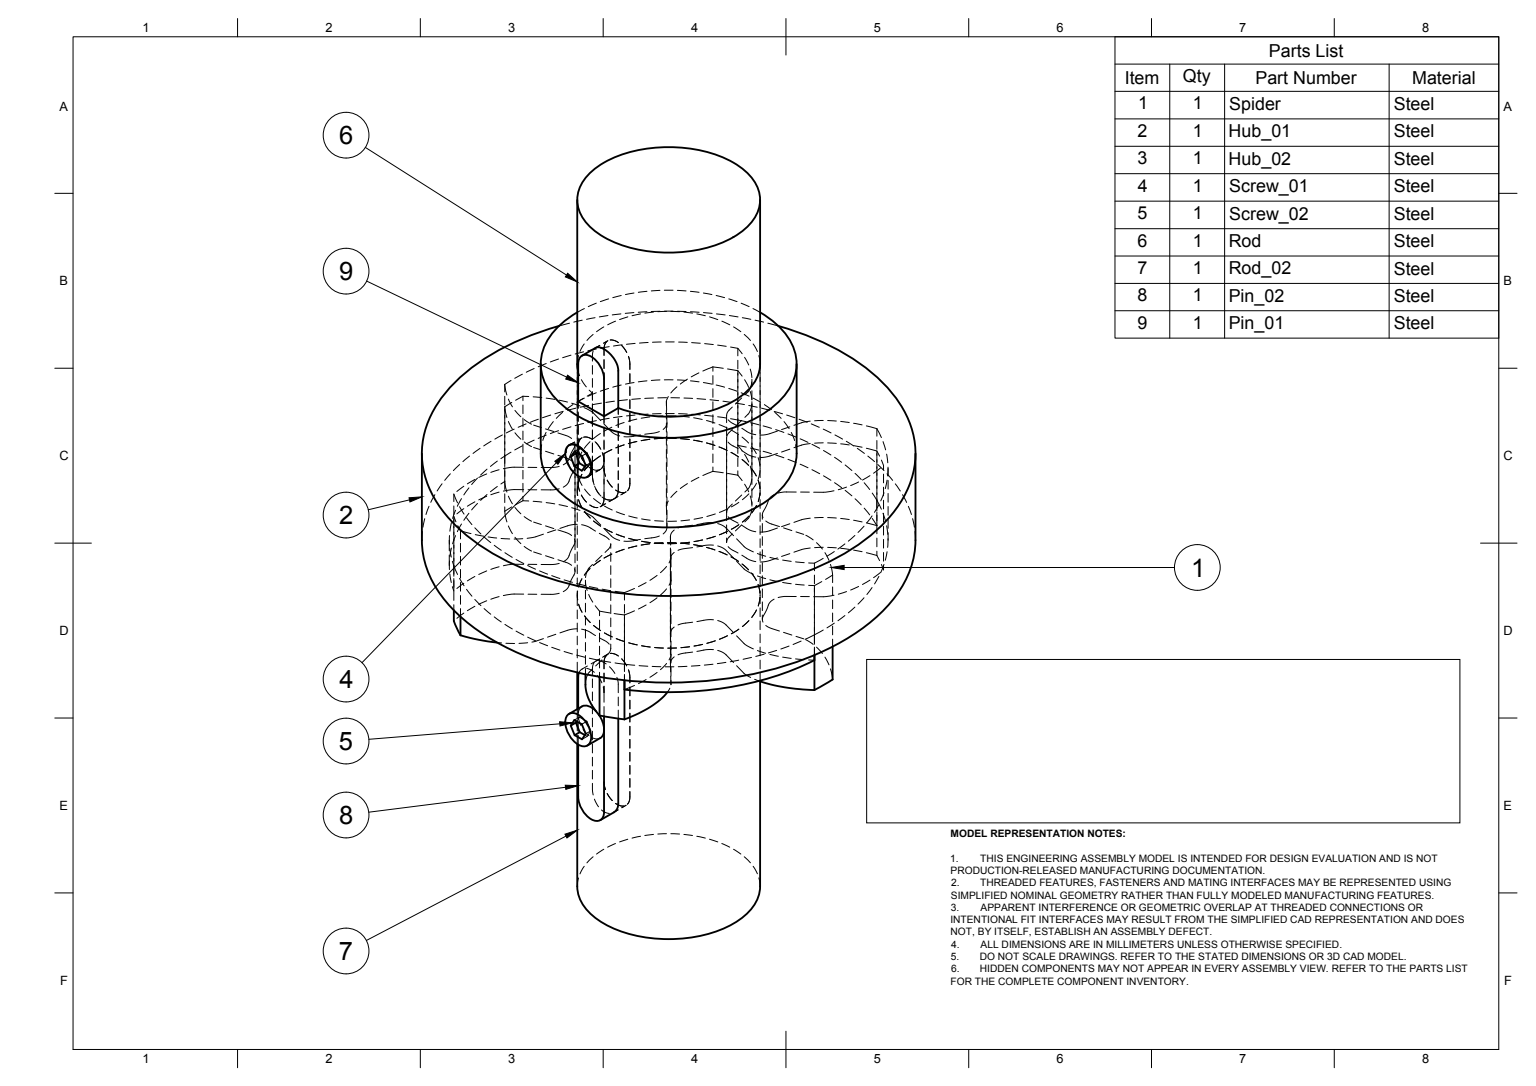
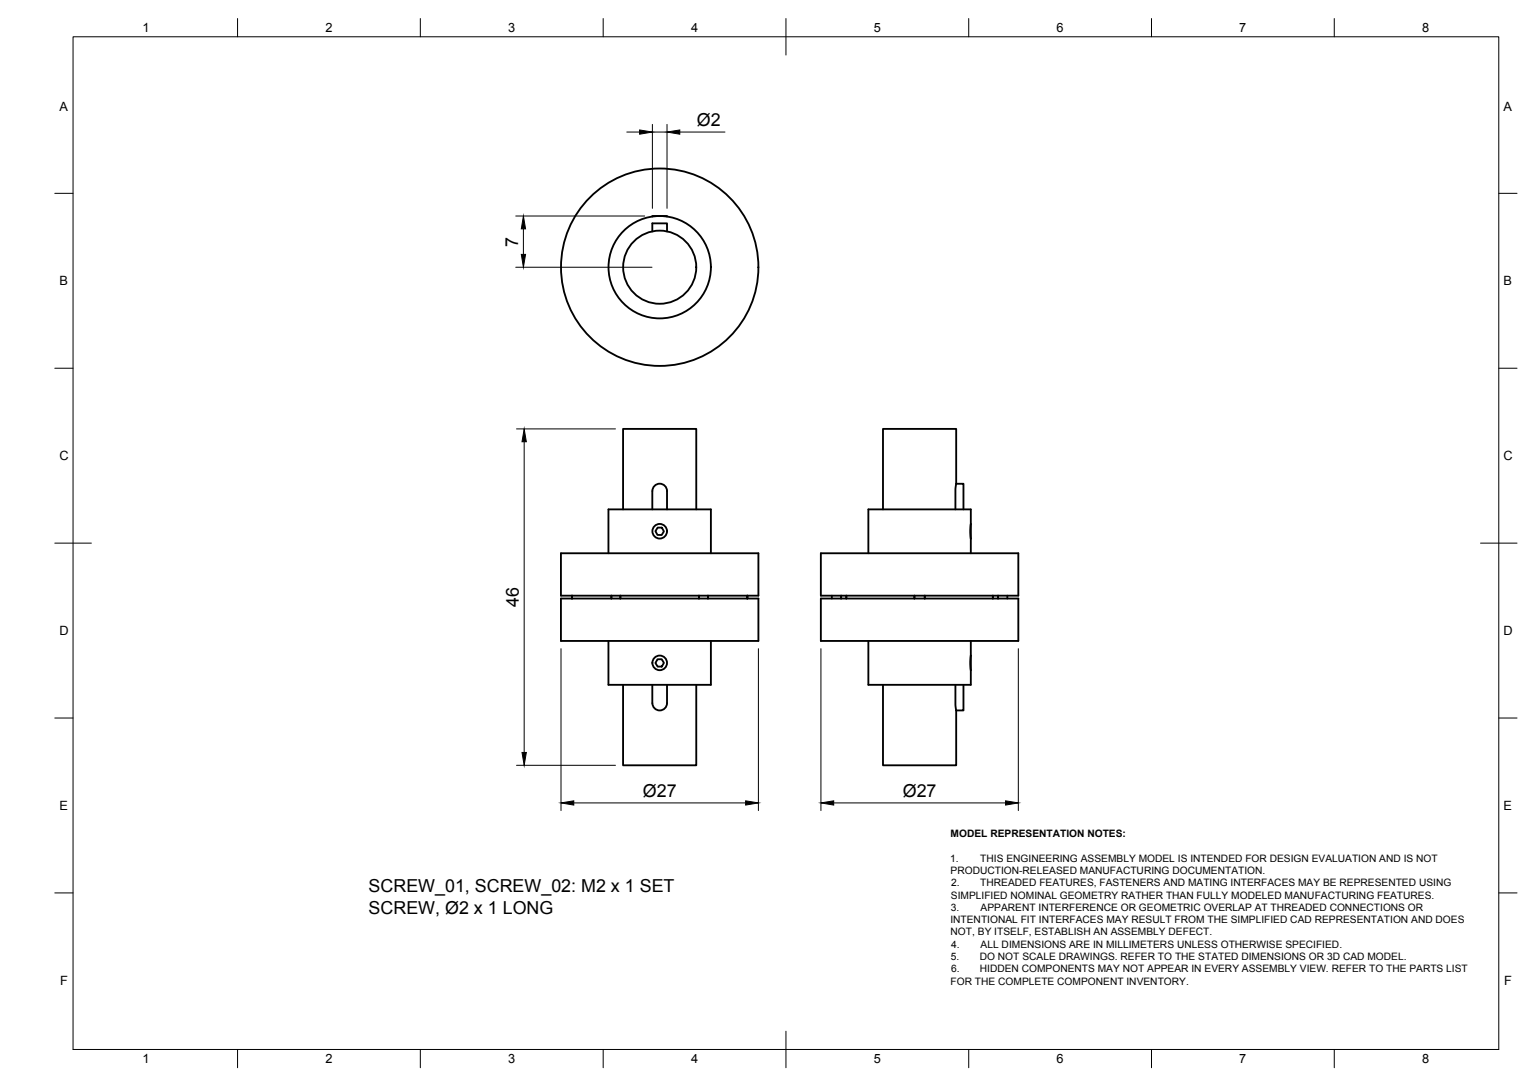
ISO-10303-21;
HEADER;
/* Generated by software containing ST-Developer
 * from STEP Tools, Inc. (www.steptools.com) 
 */

FILE_DESCRIPTION(
/* description */ (''),
/* implementation_level */ '2;1');

FILE_NAME(
/* name */ 'BR-255',
/* time_stamp */ '2026-10-05T21:34:53-07:00',
/* author */ (''),
/* organization */ (''),
/* preprocessor_version */ 'ST-DEVELOPER v20.2',
/* originating_system */ 'Autodesk Translation Framework v15.15.0.0',
/* authorisation */ '');

FILE_SCHEMA (('AUTOMOTIVE_DESIGN { 1 0 10303 214 3 1 1 }'));
ENDSEC;

DATA;
#10=MECHANICAL_DESIGN_GEOMETRIC_PRESENTATION_REPRESENTATION('',(#65,#66,
#67,#68,#69,#70,#71,#72,#73),#9822);
#11=ITEM_DEFINED_TRANSFORMATION($,$,#3398,#3718);
#12=ITEM_DEFINED_TRANSFORMATION($,$,#3488,#3719);
#13=ITEM_DEFINED_TRANSFORMATION($,$,#3566,#3720);
#14=ITEM_DEFINED_TRANSFORMATION($,$,#3644,#3721);
#15=ITEM_DEFINED_TRANSFORMATION($,$,#3657,#3722);
#16=ITEM_DEFINED_TRANSFORMATION($,$,#3670,#3723);
#17=ITEM_DEFINED_TRANSFORMATION($,$,#3683,#3724);
#18=ITEM_DEFINED_TRANSFORMATION($,$,#3696,#3725);
#19=ITEM_DEFINED_TRANSFORMATION($,$,#3707,#3726);
#20=(
REPRESENTATION_RELATIONSHIP($,$,#9857,#9856)
REPRESENTATION_RELATIONSHIP_WITH_TRANSFORMATION(#11)
SHAPE_REPRESENTATION_RELATIONSHIP()
);
#21=(
REPRESENTATION_RELATIONSHIP($,$,#9858,#9856)
REPRESENTATION_RELATIONSHIP_WITH_TRANSFORMATION(#12)
SHAPE_REPRESENTATION_RELATIONSHIP()
);
#22=(
REPRESENTATION_RELATIONSHIP($,$,#9859,#9856)
REPRESENTATION_RELATIONSHIP_WITH_TRANSFORMATION(#13)
SHAPE_REPRESENTATION_RELATIONSHIP()
);
#23=(
REPRESENTATION_RELATIONSHIP($,$,#9860,#9856)
REPRESENTATION_RELATIONSHIP_WITH_TRANSFORMATION(#14)
SHAPE_REPRESENTATION_RELATIONSHIP()
);
#24=(
REPRESENTATION_RELATIONSHIP($,$,#9861,#9856)
REPRESENTATION_RELATIONSHIP_WITH_TRANSFORMATION(#15)
SHAPE_REPRESENTATION_RELATIONSHIP()
);
#25=(
REPRESENTATION_RELATIONSHIP($,$,#9862,#9856)
REPRESENTATION_RELATIONSHIP_WITH_TRANSFORMATION(#16)
SHAPE_REPRESENTATION_RELATIONSHIP()
);
#26=(
REPRESENTATION_RELATIONSHIP($,$,#9863,#9856)
REPRESENTATION_RELATIONSHIP_WITH_TRANSFORMATION(#17)
SHAPE_REPRESENTATION_RELATIONSHIP()
);
#27=(
REPRESENTATION_RELATIONSHIP($,$,#9864,#9856)
REPRESENTATION_RELATIONSHIP_WITH_TRANSFORMATION(#18)
SHAPE_REPRESENTATION_RELATIONSHIP()
);
#28=(
REPRESENTATION_RELATIONSHIP($,$,#9865,#9856)
REPRESENTATION_RELATIONSHIP_WITH_TRANSFORMATION(#19)
SHAPE_REPRESENTATION_RELATIONSHIP()
);
#29=CONTEXT_DEPENDENT_SHAPE_REPRESENTATION(#20,#9847);
#30=CONTEXT_DEPENDENT_SHAPE_REPRESENTATION(#21,#9848);
#31=CONTEXT_DEPENDENT_SHAPE_REPRESENTATION(#22,#9849);
#32=CONTEXT_DEPENDENT_SHAPE_REPRESENTATION(#23,#9850);
#33=CONTEXT_DEPENDENT_SHAPE_REPRESENTATION(#24,#9851);
#34=CONTEXT_DEPENDENT_SHAPE_REPRESENTATION(#25,#9852);
#35=CONTEXT_DEPENDENT_SHAPE_REPRESENTATION(#26,#9853);
#36=CONTEXT_DEPENDENT_SHAPE_REPRESENTATION(#27,#9854);
#37=CONTEXT_DEPENDENT_SHAPE_REPRESENTATION(#28,#9855);
#38=NEXT_ASSEMBLY_USAGE_OCCURRENCE('Spider:1','Spider:1','Spider:1',#9867,
#9868,'Spider:1');
#39=NEXT_ASSEMBLY_USAGE_OCCURRENCE('Hub_01:1','Hub_01:1','Hub_01:1',#9867,
#9869,'Hub_01:1');
#40=NEXT_ASSEMBLY_USAGE_OCCURRENCE('Hub_02:1','Hub_02:1','Hub_02:1',#9867,
#9870,'Hub_02:1');
#41=NEXT_ASSEMBLY_USAGE_OCCURRENCE('Screw_01:1','Screw_01:1',
'Screw_01:1',#9867,#9871,'Screw_01:1');
#42=NEXT_ASSEMBLY_USAGE_OCCURRENCE('Screw_02:1','Screw_02:1',
'Screw_02:1',#9867,#9872,'Screw_02:1');
#43=NEXT_ASSEMBLY_USAGE_OCCURRENCE('Rod:1','Rod:1','Rod:1',#9867,#9873,
'Rod:1');
#44=NEXT_ASSEMBLY_USAGE_OCCURRENCE('Rod_02:1','Rod_02:1','Rod_02:1',#9867,
#9874,'Rod_02:1');
#45=NEXT_ASSEMBLY_USAGE_OCCURRENCE('Pin_02:1','Pin_02:1','Pin_02:1',#9867,
#9875,'Pin_02:1');
#46=NEXT_ASSEMBLY_USAGE_OCCURRENCE('Pin_01:1','Pin_01:1','Pin_01:1',#9867,
#9876,'Pin_01:1');
#47=SHAPE_REPRESENTATION_RELATIONSHIP('SRR','None',#9857,#56);
#48=SHAPE_REPRESENTATION_RELATIONSHIP('SRR','None',#9858,#57);
#49=SHAPE_REPRESENTATION_RELATIONSHIP('SRR','None',#9859,#58);
#50=SHAPE_REPRESENTATION_RELATIONSHIP('SRR','None',#9860,#59);
#51=SHAPE_REPRESENTATION_RELATIONSHIP('SRR','None',#9861,#60);
#52=SHAPE_REPRESENTATION_RELATIONSHIP('SRR','None',#9862,#61);
#53=SHAPE_REPRESENTATION_RELATIONSHIP('SRR','None',#9863,#62);
#54=SHAPE_REPRESENTATION_RELATIONSHIP('SRR','None',#9864,#63);
#55=SHAPE_REPRESENTATION_RELATIONSHIP('SRR','None',#9865,#64);
#56=ADVANCED_BREP_SHAPE_REPRESENTATION('',(#74),#9813);
#57=ADVANCED_BREP_SHAPE_REPRESENTATION('',(#75),#9814);
#58=ADVANCED_BREP_SHAPE_REPRESENTATION('',(#76),#9815);
#59=ADVANCED_BREP_SHAPE_REPRESENTATION('',(#77),#9816);
#60=ADVANCED_BREP_SHAPE_REPRESENTATION('',(#78),#9817);
#61=ADVANCED_BREP_SHAPE_REPRESENTATION('',(#79),#9818);
#62=ADVANCED_BREP_SHAPE_REPRESENTATION('',(#80),#9819);
#63=ADVANCED_BREP_SHAPE_REPRESENTATION('',(#81),#9820);
#64=ADVANCED_BREP_SHAPE_REPRESENTATION('',(#82),#9821);
#65=STYLED_ITEM('',(#9911),#74);
#66=STYLED_ITEM('',(#9911),#75);
#67=STYLED_ITEM('',(#9911),#76);
#68=STYLED_ITEM('',(#9912),#77);
#69=STYLED_ITEM('',(#9912),#78);
#70=STYLED_ITEM('',(#9912),#79);
#71=STYLED_ITEM('',(#9912),#80);
#72=STYLED_ITEM('',(#9912),#81);
#73=STYLED_ITEM('',(#9912),#82);
#74=MANIFOLD_SOLID_BREP('Body1',#3288);
#75=MANIFOLD_SOLID_BREP('Body1',#3289);
#76=MANIFOLD_SOLID_BREP('Body1',#3290);
#77=MANIFOLD_SOLID_BREP('Body1',#3291);
#78=MANIFOLD_SOLID_BREP('Body1',#3292);
#79=MANIFOLD_SOLID_BREP('Body1',#3293);
#80=MANIFOLD_SOLID_BREP('Body1',#3294);
#81=MANIFOLD_SOLID_BREP('Body1',#3295);
#82=MANIFOLD_SOLID_BREP('Body1',#3296);
#83=FACE_BOUND('',#486,.T.);
#84=FACE_BOUND('',#500,.T.);
#85=FACE_BOUND('',#514,.T.);
#86=FACE_BOUND('',#518,.T.);
#87=FACE_BOUND('',#520,.T.);
#88=FACE_BOUND('',#522,.T.);
#89=FACE_BOUND('',#525,.T.);
#90=FACE_BOUND('',#562,.T.);
#91=FACE_BOUND('',#566,.T.);
#92=FACE_BOUND('',#568,.T.);
#93=FACE_BOUND('',#570,.T.);
#94=FACE_BOUND('',#573,.T.);
#95=FACE_BOUND('',#608,.T.);
#96=FACE_BOUND('',#619,.T.);
#97=FACE_BOUND('',#628,.T.);
#98=FACE_BOUND('',#637,.T.);
#99=B_SPLINE_CURVE_WITH_KNOTS('',5,(#4949,#4950,#4951,#4952,#4953,#4954,
#4955,#4956,#4957,#4958,#4959,#4960,#4961,#4962,#4963,#4964,#4965,#4966,
#4967,#4968,#4969,#4970,#4971,#4972,#4973,#4974,#4975,#4976,#4977,#4978,
#4979,#4980,#4981,#4982,#4983,#4984,#4985,#4986,#4987,#4988,#4989,#4990,
#4991,#4992,#4993,#4994,#4995,#4996,#4997,#4998,#4999,#5000,#5001,#5002,
#5003,#5004,#5005,#5006,#5007,#5008,#5009,#5010,#5011,#5012,#5013,#5014,
#5015,#5016,#5017,#5018,#5019,#5020,#5021,#5022,#5023),.UNSPECIFIED.,.F.,
 .F.,(6,1,1,1,1,1,1,1,1,1,1,1,1,1,1,1,1,1,1,1,1,1,1,1,1,1,1,1,1,1,1,1,1,
1,1,1,1,1,1,1,1,1,1,1,1,1,1,1,1,1,1,1,1,1,1,1,1,1,1,1,1,1,1,1,1,1,1,1,1,
1,6),(-1.,-0.985714285714284,-0.97142857142857,-0.957142857142856,-0.942857142857141,
-0.928571428571427,-0.914285714285713,-0.899999999999999,-0.885714285714284,
-0.87142857142857,-0.857142857142856,-0.842857142857142,-0.828571428571428,
-0.814285714285713,-0.799999999999999,-0.785714285714285,-0.771428571428571,
-0.757142857142856,-0.742857142857142,-0.728571428571428,-0.714285714285714,
-0.699999999999999,-0.685714285714285,-0.671428571428571,-0.657142857142857,
-0.642857142857142,-0.628571428571428,-0.614285714285714,-0.6,-0.585714285714286,
-0.571428571428571,-0.557142857142857,-0.542857142857143,-0.528571428571429,
-0.514285714285714,-0.5,-0.485714285714286,-0.471428571428572,-0.457142857142857,
-0.442857142857143,-0.428571428571429,-0.414285714285714,-0.4,-0.385714285714286,
-0.371428571428571,-0.357142857142857,-0.342857142857143,-0.328571428571429,
-0.314285714285714,-0.3,-0.285714285714286,-0.271428571428571,-0.257142857142857,
-0.242857142857143,-0.228571428571429,-0.214285714285714,-0.2,-0.185714285714286,
-0.171428571428571,-0.157142857142857,-0.142857142857143,-0.128571428571429,
-0.114285714285714,-0.1,-0.0857142857142857,-0.0714285714285714,-0.0571428571428571,
-0.0428571428571429,-0.0285714285714286,-0.0142857142857143,0.),
 .UNSPECIFIED.);
#100=B_SPLINE_CURVE_WITH_KNOTS('',5,(#5025,#5026,#5027,#5028,#5029,#5030,
#5031,#5032,#5033,#5034,#5035,#5036,#5037,#5038,#5039,#5040,#5041,#5042,
#5043,#5044,#5045,#5046,#5047,#5048,#5049,#5050,#5051,#5052,#5053,#5054,
#5055,#5056,#5057,#5058,#5059,#5060,#5061,#5062,#5063,#5064,#5065,#5066,
#5067,#5068,#5069,#5070,#5071,#5072,#5073,#5074,#5075,#5076,#5077,#5078,
#5079,#5080,#5081,#5082,#5083,#5084,#5085,#5086,#5087,#5088,#5089,#5090,
#5091,#5092,#5093,#5094,#5095,#5096,#5097,#5098,#5099),.UNSPECIFIED.,.F.,
 .F.,(6,1,1,1,1,1,1,1,1,1,1,1,1,1,1,1,1,1,1,1,1,1,1,1,1,1,1,1,1,1,1,1,1,
1,1,1,1,1,1,1,1,1,1,1,1,1,1,1,1,1,1,1,1,1,1,1,1,1,1,1,1,1,1,1,1,1,1,1,1,
1,6),(-1.,-0.985714285714284,-0.97142857142857,-0.957142857142856,-0.942857142857141,
-0.928571428571427,-0.914285714285713,-0.899999999999999,-0.885714285714284,
-0.87142857142857,-0.857142857142856,-0.842857142857142,-0.828571428571428,
-0.814285714285713,-0.799999999999999,-0.785714285714285,-0.771428571428571,
-0.757142857142856,-0.742857142857142,-0.728571428571428,-0.714285714285714,
-0.699999999999999,-0.685714285714285,-0.671428571428571,-0.657142857142857,
-0.642857142857142,-0.628571428571428,-0.614285714285714,-0.6,-0.585714285714286,
-0.571428571428571,-0.557142857142857,-0.542857142857143,-0.528571428571429,
-0.514285714285714,-0.5,-0.485714285714286,-0.471428571428572,-0.457142857142857,
-0.442857142857143,-0.428571428571429,-0.414285714285714,-0.4,-0.385714285714286,
-0.371428571428571,-0.357142857142857,-0.342857142857143,-0.328571428571429,
-0.314285714285714,-0.3,-0.285714285714286,-0.271428571428571,-0.257142857142857,
-0.242857142857143,-0.228571428571429,-0.214285714285714,-0.2,-0.185714285714286,
-0.171428571428571,-0.157142857142857,-0.142857142857143,-0.128571428571429,
-0.114285714285714,-0.1,-0.0857142857142857,-0.0714285714285714,-0.0571428571428571,
-0.0428571428571429,-0.0285714285714286,-0.0142857142857143,0.),
 .UNSPECIFIED.);
#101=B_SPLINE_CURVE_WITH_KNOTS('',5,(#5257,#5258,#5259,#5260,#5261,#5262,
#5263,#5264,#5265,#5266,#5267,#5268,#5269,#5270,#5271,#5272,#5273,#5274,
#5275,#5276,#5277,#5278,#5279,#5280,#5281,#5282,#5283,#5284,#5285,#5286,
#5287,#5288,#5289,#5290,#5291,#5292,#5293,#5294,#5295,#5296,#5297,#5298,
#5299,#5300,#5301,#5302,#5303,#5304,#5305,#5306,#5307,#5308,#5309,#5310,
#5311,#5312,#5313,#5314,#5315,#5316,#5317,#5318,#5319,#5320,#5321,#5322,
#5323,#5324,#5325,#5326,#5327,#5328,#5329,#5330,#5331),.UNSPECIFIED.,.F.,
 .F.,(6,1,1,1,1,1,1,1,1,1,1,1,1,1,1,1,1,1,1,1,1,1,1,1,1,1,1,1,1,1,1,1,1,
1,1,1,1,1,1,1,1,1,1,1,1,1,1,1,1,1,1,1,1,1,1,1,1,1,1,1,1,1,1,1,1,1,1,1,1,
1,6),(0.,0.0142857142857143,0.0285714285714286,0.0428571428571429,0.0571428571428571,
0.0714285714285714,0.0857142857142857,0.1,0.114285714285714,0.128571428571429,
0.142857142857143,0.157142857142857,0.171428571428571,0.185714285714286,
0.2,0.214285714285714,0.228571428571429,0.242857142857143,0.257142857142857,
0.271428571428571,0.285714285714286,0.3,0.314285714285714,0.328571428571429,
0.342857142857143,0.357142857142857,0.371428571428571,0.385714285714286,
0.4,0.414285714285714,0.428571428571429,0.442857142857143,0.457142857142857,
0.471428571428572,0.485714285714286,0.5,0.514285714285714,0.528571428571429,
0.542857142857143,0.557142857142857,0.571428571428571,0.585714285714286,
0.6,0.614285714285714,0.628571428571428,0.642857142857142,0.657142857142857,
0.671428571428571,0.685714285714285,0.699999999999999,0.714285714285714,
0.728571428571428,0.742857142857142,0.757142857142856,0.771428571428571,
0.785714285714285,0.799999999999999,0.814285714285713,0.828571428571428,
0.842857142857142,0.857142857142856,0.87142857142857,0.885714285714284,
0.899999999999999,0.914285714285713,0.928571428571427,0.942857142857141,
0.957142857142856,0.97142857142857,0.985714285714284,1.),.UNSPECIFIED.);
#102=B_SPLINE_CURVE_WITH_KNOTS('',5,(#5332,#5333,#5334,#5335,#5336,#5337,
#5338,#5339,#5340,#5341,#5342,#5343,#5344,#5345,#5346,#5347,#5348,#5349,
#5350,#5351,#5352,#5353,#5354,#5355,#5356,#5357,#5358,#5359,#5360,#5361,
#5362,#5363,#5364,#5365,#5366,#5367,#5368,#5369,#5370,#5371,#5372,#5373,
#5374,#5375,#5376,#5377,#5378,#5379,#5380,#5381,#5382,#5383,#5384,#5385,
#5386,#5387,#5388,#5389,#5390,#5391,#5392,#5393,#5394,#5395,#5396,#5397,
#5398,#5399,#5400,#5401,#5402,#5403,#5404,#5405,#5406),.UNSPECIFIED.,.F.,
 .F.,(6,1,1,1,1,1,1,1,1,1,1,1,1,1,1,1,1,1,1,1,1,1,1,1,1,1,1,1,1,1,1,1,1,
1,1,1,1,1,1,1,1,1,1,1,1,1,1,1,1,1,1,1,1,1,1,1,1,1,1,1,1,1,1,1,1,1,1,1,1,
1,6),(0.,0.0142857142857143,0.0285714285714286,0.0428571428571429,0.0571428571428571,
0.0714285714285714,0.0857142857142857,0.1,0.114285714285714,0.128571428571429,
0.142857142857143,0.157142857142857,0.171428571428571,0.185714285714286,
0.2,0.214285714285714,0.228571428571429,0.242857142857143,0.257142857142857,
0.271428571428571,0.285714285714286,0.3,0.314285714285714,0.328571428571429,
0.342857142857143,0.357142857142857,0.371428571428571,0.385714285714286,
0.4,0.414285714285714,0.428571428571429,0.442857142857143,0.457142857142857,
0.471428571428572,0.485714285714286,0.5,0.514285714285714,0.528571428571429,
0.542857142857143,0.557142857142857,0.571428571428571,0.585714285714286,
0.6,0.614285714285714,0.628571428571428,0.642857142857142,0.657142857142857,
0.671428571428571,0.685714285714285,0.699999999999999,0.714285714285714,
0.728571428571428,0.742857142857142,0.757142857142856,0.771428571428571,
0.785714285714285,0.799999999999999,0.814285714285713,0.828571428571428,
0.842857142857142,0.857142857142856,0.87142857142857,0.885714285714284,
0.899999999999999,0.914285714285713,0.928571428571427,0.942857142857141,
0.957142857142856,0.97142857142857,0.985714285714284,1.),.UNSPECIFIED.);
#103=B_SPLINE_CURVE_WITH_KNOTS('',5,(#5558,#5559,#5560,#5561,#5562,#5563,
#5564,#5565,#5566,#5567,#5568,#5569,#5570,#5571,#5572,#5573,#5574,#5575,
#5576,#5577,#5578,#5579,#5580,#5581,#5582,#5583,#5584,#5585,#5586,#5587,
#5588,#5589,#5590,#5591,#5592,#5593,#5594,#5595,#5596,#5597,#5598,#5599,
#5600,#5601,#5602,#5603,#5604,#5605,#5606,#5607,#5608,#5609,#5610,#5611,
#5612,#5613,#5614,#5615,#5616,#5617,#5618,#5619,#5620,#5621,#5622,#5623,
#5624,#5625,#5626,#5627,#5628,#5629,#5630,#5631,#5632),.UNSPECIFIED.,.F.,
 .F.,(6,1,1,1,1,1,1,1,1,1,1,1,1,1,1,1,1,1,1,1,1,1,1,1,1,1,1,1,1,1,1,1,1,
1,1,1,1,1,1,1,1,1,1,1,1,1,1,1,1,1,1,1,1,1,1,1,1,1,1,1,1,1,1,1,1,1,1,1,1,
1,6),(-1.,-0.985714285714284,-0.97142857142857,-0.957142857142856,-0.942857142857141,
-0.928571428571427,-0.914285714285713,-0.899999999999999,-0.885714285714284,
-0.87142857142857,-0.857142857142856,-0.842857142857142,-0.828571428571428,
-0.814285714285713,-0.799999999999999,-0.785714285714285,-0.771428571428571,
-0.757142857142856,-0.742857142857142,-0.728571428571428,-0.714285714285714,
-0.699999999999999,-0.685714285714285,-0.671428571428571,-0.657142857142857,
-0.642857142857142,-0.628571428571428,-0.614285714285714,-0.6,-0.585714285714286,
-0.571428571428571,-0.557142857142857,-0.542857142857143,-0.528571428571429,
-0.514285714285714,-0.5,-0.485714285714286,-0.471428571428572,-0.457142857142857,
-0.442857142857143,-0.428571428571429,-0.414285714285714,-0.4,-0.385714285714286,
-0.371428571428571,-0.357142857142857,-0.342857142857143,-0.328571428571429,
-0.314285714285714,-0.3,-0.285714285714286,-0.271428571428571,-0.257142857142857,
-0.242857142857143,-0.228571428571429,-0.214285714285714,-0.2,-0.185714285714286,
-0.171428571428571,-0.157142857142857,-0.142857142857143,-0.128571428571429,
-0.114285714285714,-0.1,-0.0857142857142857,-0.0714285714285714,-0.0571428571428571,
-0.0428571428571429,-0.0285714285714286,-0.0142857142857143,0.),
 .UNSPECIFIED.);
#104=B_SPLINE_CURVE_WITH_KNOTS('',5,(#5634,#5635,#5636,#5637,#5638,#5639,
#5640,#5641,#5642,#5643,#5644,#5645,#5646,#5647,#5648,#5649,#5650,#5651,
#5652,#5653,#5654,#5655,#5656,#5657,#5658,#5659,#5660,#5661,#5662,#5663,
#5664,#5665,#5666,#5667,#5668,#5669,#5670,#5671,#5672,#5673,#5674,#5675,
#5676,#5677,#5678,#5679,#5680,#5681,#5682,#5683,#5684,#5685,#5686,#5687,
#5688,#5689,#5690,#5691,#5692,#5693,#5694,#5695,#5696,#5697,#5698,#5699,
#5700,#5701,#5702,#5703,#5704,#5705,#5706,#5707,#5708),.UNSPECIFIED.,.F.,
 .F.,(6,1,1,1,1,1,1,1,1,1,1,1,1,1,1,1,1,1,1,1,1,1,1,1,1,1,1,1,1,1,1,1,1,
1,1,1,1,1,1,1,1,1,1,1,1,1,1,1,1,1,1,1,1,1,1,1,1,1,1,1,1,1,1,1,1,1,1,1,1,
1,6),(-1.,-0.985714285714284,-0.97142857142857,-0.957142857142856,-0.942857142857141,
-0.928571428571427,-0.914285714285713,-0.899999999999999,-0.885714285714284,
-0.87142857142857,-0.857142857142856,-0.842857142857142,-0.828571428571428,
-0.814285714285713,-0.799999999999999,-0.785714285714285,-0.771428571428571,
-0.757142857142856,-0.742857142857142,-0.728571428571428,-0.714285714285714,
-0.699999999999999,-0.685714285714285,-0.671428571428571,-0.657142857142857,
-0.642857142857142,-0.628571428571428,-0.614285714285714,-0.6,-0.585714285714286,
-0.571428571428571,-0.557142857142857,-0.542857142857143,-0.528571428571429,
-0.514285714285714,-0.5,-0.485714285714286,-0.471428571428572,-0.457142857142857,
-0.442857142857143,-0.428571428571429,-0.414285714285714,-0.4,-0.385714285714286,
-0.371428571428571,-0.357142857142857,-0.342857142857143,-0.328571428571429,
-0.314285714285714,-0.3,-0.285714285714286,-0.271428571428571,-0.257142857142857,
-0.242857142857143,-0.228571428571429,-0.214285714285714,-0.2,-0.185714285714286,
-0.171428571428571,-0.157142857142857,-0.142857142857143,-0.128571428571429,
-0.114285714285714,-0.1,-0.0857142857142857,-0.0714285714285714,-0.0571428571428571,
-0.0428571428571429,-0.0285714285714286,-0.0142857142857143,0.),
 .UNSPECIFIED.);
#105=B_SPLINE_CURVE_WITH_KNOTS('',5,(#5866,#5867,#5868,#5869,#5870,#5871,
#5872,#5873,#5874,#5875,#5876,#5877,#5878,#5879,#5880,#5881,#5882,#5883,
#5884,#5885,#5886,#5887,#5888,#5889,#5890,#5891,#5892,#5893,#5894,#5895,
#5896,#5897,#5898,#5899,#5900,#5901,#5902,#5903,#5904,#5905,#5906,#5907,
#5908,#5909,#5910,#5911,#5912,#5913,#5914,#5915,#5916,#5917,#5918,#5919,
#5920,#5921,#5922,#5923,#5924,#5925,#5926,#5927,#5928,#5929,#5930,#5931,
#5932,#5933,#5934,#5935,#5936,#5937,#5938,#5939,#5940),.UNSPECIFIED.,.F.,
 .F.,(6,1,1,1,1,1,1,1,1,1,1,1,1,1,1,1,1,1,1,1,1,1,1,1,1,1,1,1,1,1,1,1,1,
1,1,1,1,1,1,1,1,1,1,1,1,1,1,1,1,1,1,1,1,1,1,1,1,1,1,1,1,1,1,1,1,1,1,1,1,
1,6),(0.,0.0142857142857143,0.0285714285714286,0.0428571428571429,0.0571428571428571,
0.0714285714285714,0.0857142857142857,0.1,0.114285714285714,0.128571428571429,
0.142857142857143,0.157142857142857,0.171428571428571,0.185714285714286,
0.2,0.214285714285714,0.228571428571429,0.242857142857143,0.257142857142857,
0.271428571428571,0.285714285714286,0.3,0.314285714285714,0.328571428571429,
0.342857142857143,0.357142857142857,0.371428571428571,0.385714285714286,
0.4,0.414285714285714,0.428571428571429,0.442857142857143,0.457142857142857,
0.471428571428572,0.485714285714286,0.5,0.514285714285714,0.528571428571429,
0.542857142857143,0.557142857142857,0.571428571428571,0.585714285714286,
0.6,0.614285714285714,0.628571428571428,0.642857142857142,0.657142857142857,
0.671428571428571,0.685714285714285,0.699999999999999,0.714285714285714,
0.728571428571428,0.742857142857142,0.757142857142856,0.771428571428571,
0.785714285714285,0.799999999999999,0.814285714285713,0.828571428571428,
0.842857142857142,0.857142857142856,0.87142857142857,0.885714285714284,
0.899999999999999,0.914285714285713,0.928571428571427,0.942857142857141,
0.957142857142856,0.97142857142857,0.985714285714284,1.),.UNSPECIFIED.);
#106=B_SPLINE_CURVE_WITH_KNOTS('',5,(#5941,#5942,#5943,#5944,#5945,#5946,
#5947,#5948,#5949,#5950,#5951,#5952,#5953,#5954,#5955,#5956,#5957,#5958,
#5959,#5960,#5961,#5962,#5963,#5964,#5965,#5966,#5967,#5968,#5969,#5970,
#5971,#5972,#5973,#5974,#5975,#5976,#5977,#5978,#5979,#5980,#5981,#5982,
#5983,#5984,#5985,#5986,#5987,#5988,#5989,#5990,#5991,#5992,#5993,#5994,
#5995,#5996,#5997,#5998,#5999,#6000,#6001,#6002,#6003,#6004,#6005,#6006,
#6007,#6008,#6009,#6010,#6011,#6012,#6013,#6014,#6015),.UNSPECIFIED.,.F.,
 .F.,(6,1,1,1,1,1,1,1,1,1,1,1,1,1,1,1,1,1,1,1,1,1,1,1,1,1,1,1,1,1,1,1,1,
1,1,1,1,1,1,1,1,1,1,1,1,1,1,1,1,1,1,1,1,1,1,1,1,1,1,1,1,1,1,1,1,1,1,1,1,
1,6),(0.,0.0142857142857143,0.0285714285714286,0.0428571428571429,0.0571428571428571,
0.0714285714285714,0.0857142857142857,0.1,0.114285714285714,0.128571428571429,
0.142857142857143,0.157142857142857,0.171428571428571,0.185714285714286,
0.2,0.214285714285714,0.228571428571429,0.242857142857143,0.257142857142857,
0.271428571428571,0.285714285714286,0.3,0.314285714285714,0.328571428571429,
0.342857142857143,0.357142857142857,0.371428571428571,0.385714285714286,
0.4,0.414285714285714,0.428571428571429,0.442857142857143,0.457142857142857,
0.471428571428572,0.485714285714286,0.5,0.514285714285714,0.528571428571429,
0.542857142857143,0.557142857142857,0.571428571428571,0.585714285714286,
0.6,0.614285714285714,0.628571428571428,0.642857142857142,0.657142857142857,
0.671428571428571,0.685714285714285,0.699999999999999,0.714285714285714,
0.728571428571428,0.742857142857142,0.757142857142856,0.771428571428571,
0.785714285714285,0.799999999999999,0.814285714285713,0.828571428571428,
0.842857142857142,0.857142857142856,0.87142857142857,0.885714285714284,
0.899999999999999,0.914285714285713,0.928571428571427,0.942857142857141,
0.957142857142856,0.97142857142857,0.985714285714284,1.),.UNSPECIFIED.);
#107=B_SPLINE_CURVE_WITH_KNOTS('',5,(#6167,#6168,#6169,#6170,#6171,#6172,
#6173,#6174,#6175,#6176,#6177,#6178,#6179,#6180,#6181,#6182,#6183,#6184,
#6185,#6186,#6187,#6188,#6189,#6190,#6191,#6192,#6193,#6194,#6195,#6196,
#6197,#6198,#6199,#6200,#6201,#6202,#6203,#6204,#6205,#6206,#6207,#6208,
#6209,#6210,#6211,#6212,#6213,#6214,#6215,#6216,#6217,#6218,#6219,#6220,
#6221,#6222,#6223,#6224,#6225,#6226,#6227,#6228,#6229,#6230,#6231,#6232,
#6233,#6234,#6235,#6236,#6237,#6238,#6239,#6240,#6241),.UNSPECIFIED.,.F.,
 .F.,(6,1,1,1,1,1,1,1,1,1,1,1,1,1,1,1,1,1,1,1,1,1,1,1,1,1,1,1,1,1,1,1,1,
1,1,1,1,1,1,1,1,1,1,1,1,1,1,1,1,1,1,1,1,1,1,1,1,1,1,1,1,1,1,1,1,1,1,1,1,
1,6),(-1.,-0.985714285714284,-0.97142857142857,-0.957142857142856,-0.942857142857141,
-0.928571428571427,-0.914285714285713,-0.899999999999999,-0.885714285714284,
-0.87142857142857,-0.857142857142856,-0.842857142857142,-0.828571428571428,
-0.814285714285713,-0.799999999999999,-0.785714285714285,-0.771428571428571,
-0.757142857142856,-0.742857142857142,-0.728571428571428,-0.714285714285714,
-0.699999999999999,-0.685714285714285,-0.671428571428571,-0.657142857142857,
-0.642857142857142,-0.628571428571428,-0.614285714285714,-0.6,-0.585714285714286,
-0.571428571428571,-0.557142857142857,-0.542857142857143,-0.528571428571429,
-0.514285714285714,-0.5,-0.485714285714286,-0.471428571428572,-0.457142857142857,
-0.442857142857143,-0.428571428571429,-0.414285714285714,-0.4,-0.385714285714286,
-0.371428571428571,-0.357142857142857,-0.342857142857143,-0.328571428571429,
-0.314285714285714,-0.3,-0.285714285714286,-0.271428571428571,-0.257142857142857,
-0.242857142857143,-0.228571428571429,-0.214285714285714,-0.2,-0.185714285714286,
-0.171428571428571,-0.157142857142857,-0.142857142857143,-0.128571428571429,
-0.114285714285714,-0.1,-0.0857142857142857,-0.0714285714285714,-0.0571428571428571,
-0.0428571428571429,-0.0285714285714286,-0.0142857142857143,0.),
 .UNSPECIFIED.);
#108=B_SPLINE_CURVE_WITH_KNOTS('',5,(#6243,#6244,#6245,#6246,#6247,#6248,
#6249,#6250,#6251,#6252,#6253,#6254,#6255,#6256,#6257,#6258,#6259,#6260,
#6261,#6262,#6263,#6264,#6265,#6266,#6267,#6268,#6269,#6270,#6271,#6272,
#6273,#6274,#6275,#6276,#6277,#6278,#6279,#6280,#6281,#6282,#6283,#6284,
#6285,#6286,#6287,#6288,#6289,#6290,#6291,#6292,#6293,#6294,#6295,#6296,
#6297,#6298,#6299,#6300,#6301,#6302,#6303,#6304,#6305,#6306,#6307,#6308,
#6309,#6310,#6311,#6312,#6313,#6314,#6315,#6316,#6317),.UNSPECIFIED.,.F.,
 .F.,(6,1,1,1,1,1,1,1,1,1,1,1,1,1,1,1,1,1,1,1,1,1,1,1,1,1,1,1,1,1,1,1,1,
1,1,1,1,1,1,1,1,1,1,1,1,1,1,1,1,1,1,1,1,1,1,1,1,1,1,1,1,1,1,1,1,1,1,1,1,
1,6),(-1.,-0.985714285714284,-0.97142857142857,-0.957142857142856,-0.942857142857141,
-0.928571428571427,-0.914285714285713,-0.899999999999999,-0.885714285714284,
-0.87142857142857,-0.857142857142856,-0.842857142857142,-0.828571428571428,
-0.814285714285713,-0.799999999999999,-0.785714285714285,-0.771428571428571,
-0.757142857142856,-0.742857142857142,-0.728571428571428,-0.714285714285714,
-0.699999999999999,-0.685714285714285,-0.671428571428571,-0.657142857142857,
-0.642857142857142,-0.628571428571428,-0.614285714285714,-0.6,-0.585714285714286,
-0.571428571428571,-0.557142857142857,-0.542857142857143,-0.528571428571429,
-0.514285714285714,-0.5,-0.485714285714286,-0.471428571428572,-0.457142857142857,
-0.442857142857143,-0.428571428571429,-0.414285714285714,-0.4,-0.385714285714286,
-0.371428571428571,-0.357142857142857,-0.342857142857143,-0.328571428571429,
-0.314285714285714,-0.3,-0.285714285714286,-0.271428571428571,-0.257142857142857,
-0.242857142857143,-0.228571428571429,-0.214285714285714,-0.2,-0.185714285714286,
-0.171428571428571,-0.157142857142857,-0.142857142857143,-0.128571428571429,
-0.114285714285714,-0.1,-0.0857142857142857,-0.0714285714285714,-0.0571428571428571,
-0.0428571428571429,-0.0285714285714286,-0.0142857142857143,0.),
 .UNSPECIFIED.);
#109=B_SPLINE_CURVE_WITH_KNOTS('',5,(#6475,#6476,#6477,#6478,#6479,#6480,
#6481,#6482,#6483,#6484,#6485,#6486,#6487,#6488,#6489,#6490,#6491,#6492,
#6493,#6494,#6495,#6496,#6497,#6498,#6499,#6500,#6501,#6502,#6503,#6504,
#6505,#6506,#6507,#6508,#6509,#6510,#6511,#6512,#6513,#6514,#6515,#6516,
#6517,#6518,#6519,#6520,#6521,#6522,#6523,#6524,#6525,#6526,#6527,#6528,
#6529,#6530,#6531,#6532,#6533,#6534,#6535,#6536,#6537,#6538,#6539,#6540,
#6541,#6542,#6543,#6544,#6545,#6546,#6547,#6548,#6549),.UNSPECIFIED.,.F.,
 .F.,(6,1,1,1,1,1,1,1,1,1,1,1,1,1,1,1,1,1,1,1,1,1,1,1,1,1,1,1,1,1,1,1,1,
1,1,1,1,1,1,1,1,1,1,1,1,1,1,1,1,1,1,1,1,1,1,1,1,1,1,1,1,1,1,1,1,1,1,1,1,
1,6),(0.,0.0142857142857143,0.0285714285714286,0.0428571428571429,0.0571428571428571,
0.0714285714285714,0.0857142857142857,0.1,0.114285714285714,0.128571428571429,
0.142857142857143,0.157142857142857,0.171428571428571,0.185714285714286,
0.2,0.214285714285714,0.228571428571429,0.242857142857143,0.257142857142857,
0.271428571428571,0.285714285714286,0.3,0.314285714285714,0.328571428571429,
0.342857142857143,0.357142857142857,0.371428571428571,0.385714285714286,
0.4,0.414285714285714,0.428571428571429,0.442857142857143,0.457142857142857,
0.471428571428572,0.485714285714286,0.5,0.514285714285714,0.528571428571429,
0.542857142857143,0.557142857142857,0.571428571428571,0.585714285714286,
0.6,0.614285714285714,0.628571428571428,0.642857142857142,0.657142857142857,
0.671428571428571,0.685714285714285,0.699999999999999,0.714285714285714,
0.728571428571428,0.742857142857142,0.757142857142856,0.771428571428571,
0.785714285714285,0.799999999999999,0.814285714285713,0.828571428571428,
0.842857142857142,0.857142857142856,0.87142857142857,0.885714285714284,
0.899999999999999,0.914285714285713,0.928571428571427,0.942857142857141,
0.957142857142856,0.97142857142857,0.985714285714284,1.),.UNSPECIFIED.);
#110=B_SPLINE_CURVE_WITH_KNOTS('',5,(#6550,#6551,#6552,#6553,#6554,#6555,
#6556,#6557,#6558,#6559,#6560,#6561,#6562,#6563,#6564,#6565,#6566,#6567,
#6568,#6569,#6570,#6571,#6572,#6573,#6574,#6575,#6576,#6577,#6578,#6579,
#6580,#6581,#6582,#6583,#6584,#6585,#6586,#6587,#6588,#6589,#6590,#6591,
#6592,#6593,#6594,#6595,#6596,#6597,#6598,#6599,#6600,#6601,#6602,#6603,
#6604,#6605,#6606,#6607,#6608,#6609,#6610,#6611,#6612,#6613,#6614,#6615,
#6616,#6617,#6618,#6619,#6620,#6621,#6622,#6623,#6624),.UNSPECIFIED.,.F.,
 .F.,(6,1,1,1,1,1,1,1,1,1,1,1,1,1,1,1,1,1,1,1,1,1,1,1,1,1,1,1,1,1,1,1,1,
1,1,1,1,1,1,1,1,1,1,1,1,1,1,1,1,1,1,1,1,1,1,1,1,1,1,1,1,1,1,1,1,1,1,1,1,
1,6),(0.,0.0142857142857143,0.0285714285714286,0.0428571428571429,0.0571428571428571,
0.0714285714285714,0.0857142857142857,0.1,0.114285714285714,0.128571428571429,
0.142857142857143,0.157142857142857,0.171428571428571,0.185714285714286,
0.2,0.214285714285714,0.228571428571429,0.242857142857143,0.257142857142857,
0.271428571428571,0.285714285714286,0.3,0.314285714285714,0.328571428571429,
0.342857142857143,0.357142857142857,0.371428571428571,0.385714285714286,
0.4,0.414285714285714,0.428571428571429,0.442857142857143,0.457142857142857,
0.471428571428572,0.485714285714286,0.5,0.514285714285714,0.528571428571429,
0.542857142857143,0.557142857142857,0.571428571428571,0.585714285714286,
0.6,0.614285714285714,0.628571428571428,0.642857142857142,0.657142857142857,
0.671428571428571,0.685714285714285,0.699999999999999,0.714285714285714,
0.728571428571428,0.742857142857142,0.757142857142856,0.771428571428571,
0.785714285714285,0.799999999999999,0.814285714285713,0.828571428571428,
0.842857142857142,0.857142857142856,0.87142857142857,0.885714285714284,
0.899999999999999,0.914285714285713,0.928571428571427,0.942857142857141,
0.957142857142856,0.97142857142857,0.985714285714284,1.),.UNSPECIFIED.);
#111=B_SPLINE_CURVE_WITH_KNOTS('',5,(#6776,#6777,#6778,#6779,#6780,#6781,
#6782,#6783,#6784,#6785,#6786,#6787,#6788,#6789,#6790,#6791,#6792,#6793,
#6794,#6795,#6796,#6797,#6798,#6799,#6800,#6801,#6802,#6803,#6804,#6805,
#6806,#6807,#6808,#6809,#6810,#6811,#6812,#6813,#6814,#6815,#6816,#6817,
#6818,#6819,#6820,#6821,#6822,#6823,#6824,#6825,#6826,#6827,#6828,#6829,
#6830,#6831,#6832,#6833,#6834,#6835,#6836,#6837,#6838,#6839,#6840,#6841,
#6842,#6843,#6844,#6845,#6846,#6847,#6848,#6849,#6850),.UNSPECIFIED.,.F.,
 .F.,(6,1,1,1,1,1,1,1,1,1,1,1,1,1,1,1,1,1,1,1,1,1,1,1,1,1,1,1,1,1,1,1,1,
1,1,1,1,1,1,1,1,1,1,1,1,1,1,1,1,1,1,1,1,1,1,1,1,1,1,1,1,1,1,1,1,1,1,1,1,
1,6),(-1.,-0.985714285714284,-0.97142857142857,-0.957142857142856,-0.942857142857141,
-0.928571428571427,-0.914285714285713,-0.899999999999999,-0.885714285714284,
-0.87142857142857,-0.857142857142856,-0.842857142857142,-0.828571428571428,
-0.814285714285713,-0.799999999999999,-0.785714285714285,-0.771428571428571,
-0.757142857142856,-0.742857142857142,-0.728571428571428,-0.714285714285714,
-0.699999999999999,-0.685714285714285,-0.671428571428571,-0.657142857142857,
-0.642857142857142,-0.628571428571428,-0.614285714285714,-0.6,-0.585714285714286,
-0.571428571428571,-0.557142857142857,-0.542857142857143,-0.528571428571429,
-0.514285714285714,-0.5,-0.485714285714286,-0.471428571428572,-0.457142857142857,
-0.442857142857143,-0.428571428571429,-0.414285714285714,-0.4,-0.385714285714286,
-0.371428571428571,-0.357142857142857,-0.342857142857143,-0.328571428571429,
-0.314285714285714,-0.3,-0.285714285714286,-0.271428571428571,-0.257142857142857,
-0.242857142857143,-0.228571428571429,-0.214285714285714,-0.2,-0.185714285714286,
-0.171428571428571,-0.157142857142857,-0.142857142857143,-0.128571428571429,
-0.114285714285714,-0.1,-0.0857142857142857,-0.0714285714285714,-0.0571428571428571,
-0.0428571428571429,-0.0285714285714286,-0.0142857142857143,0.),
 .UNSPECIFIED.);
#112=B_SPLINE_CURVE_WITH_KNOTS('',5,(#6852,#6853,#6854,#6855,#6856,#6857,
#6858,#6859,#6860,#6861,#6862,#6863,#6864,#6865,#6866,#6867,#6868,#6869,
#6870,#6871,#6872,#6873,#6874,#6875,#6876,#6877,#6878,#6879,#6880,#6881,
#6882,#6883,#6884,#6885,#6886,#6887,#6888,#6889,#6890,#6891,#6892,#6893,
#6894,#6895,#6896,#6897,#6898,#6899,#6900,#6901,#6902,#6903,#6904,#6905,
#6906,#6907,#6908,#6909,#6910,#6911,#6912,#6913,#6914,#6915,#6916,#6917,
#6918,#6919,#6920,#6921,#6922,#6923,#6924,#6925,#6926),.UNSPECIFIED.,.F.,
 .F.,(6,1,1,1,1,1,1,1,1,1,1,1,1,1,1,1,1,1,1,1,1,1,1,1,1,1,1,1,1,1,1,1,1,
1,1,1,1,1,1,1,1,1,1,1,1,1,1,1,1,1,1,1,1,1,1,1,1,1,1,1,1,1,1,1,1,1,1,1,1,
1,6),(-1.,-0.985714285714284,-0.97142857142857,-0.957142857142856,-0.942857142857141,
-0.928571428571427,-0.914285714285713,-0.899999999999999,-0.885714285714284,
-0.87142857142857,-0.857142857142856,-0.842857142857142,-0.828571428571428,
-0.814285714285713,-0.799999999999999,-0.785714285714285,-0.771428571428571,
-0.757142857142856,-0.742857142857142,-0.728571428571428,-0.714285714285714,
-0.699999999999999,-0.685714285714285,-0.671428571428571,-0.657142857142857,
-0.642857142857142,-0.628571428571428,-0.614285714285714,-0.6,-0.585714285714286,
-0.571428571428571,-0.557142857142857,-0.542857142857143,-0.528571428571429,
-0.514285714285714,-0.5,-0.485714285714286,-0.471428571428572,-0.457142857142857,
-0.442857142857143,-0.428571428571429,-0.414285714285714,-0.4,-0.385714285714286,
-0.371428571428571,-0.357142857142857,-0.342857142857143,-0.328571428571429,
-0.314285714285714,-0.3,-0.285714285714286,-0.271428571428571,-0.257142857142857,
-0.242857142857143,-0.228571428571429,-0.214285714285714,-0.2,-0.185714285714286,
-0.171428571428571,-0.157142857142857,-0.142857142857143,-0.128571428571429,
-0.114285714285714,-0.1,-0.0857142857142857,-0.0714285714285714,-0.0571428571428571,
-0.0428571428571429,-0.0285714285714286,-0.0142857142857143,0.),
 .UNSPECIFIED.);
#113=B_SPLINE_CURVE_WITH_KNOTS('',5,(#7084,#7085,#7086,#7087,#7088,#7089,
#7090,#7091,#7092,#7093,#7094,#7095,#7096,#7097,#7098,#7099,#7100,#7101,
#7102,#7103,#7104,#7105,#7106,#7107,#7108,#7109,#7110,#7111,#7112,#7113,
#7114,#7115,#7116,#7117,#7118,#7119,#7120,#7121,#7122,#7123,#7124,#7125,
#7126,#7127,#7128,#7129,#7130,#7131,#7132,#7133,#7134,#7135,#7136,#7137,
#7138,#7139,#7140,#7141,#7142,#7143,#7144,#7145,#7146,#7147,#7148,#7149,
#7150,#7151,#7152,#7153,#7154,#7155,#7156,#7157,#7158),.UNSPECIFIED.,.F.,
 .F.,(6,1,1,1,1,1,1,1,1,1,1,1,1,1,1,1,1,1,1,1,1,1,1,1,1,1,1,1,1,1,1,1,1,
1,1,1,1,1,1,1,1,1,1,1,1,1,1,1,1,1,1,1,1,1,1,1,1,1,1,1,1,1,1,1,1,1,1,1,1,
1,6),(0.,0.0142857142857143,0.0285714285714286,0.0428571428571429,0.0571428571428571,
0.0714285714285714,0.0857142857142857,0.1,0.114285714285714,0.128571428571429,
0.142857142857143,0.157142857142857,0.171428571428571,0.185714285714286,
0.2,0.214285714285714,0.228571428571429,0.242857142857143,0.257142857142857,
0.271428571428571,0.285714285714286,0.3,0.314285714285714,0.328571428571429,
0.342857142857143,0.357142857142857,0.371428571428571,0.385714285714286,
0.4,0.414285714285714,0.428571428571429,0.442857142857143,0.457142857142857,
0.471428571428572,0.485714285714286,0.5,0.514285714285714,0.528571428571429,
0.542857142857143,0.557142857142857,0.571428571428571,0.585714285714286,
0.6,0.614285714285714,0.628571428571428,0.642857142857142,0.657142857142857,
0.671428571428571,0.685714285714285,0.699999999999999,0.714285714285714,
0.728571428571428,0.742857142857142,0.757142857142856,0.771428571428571,
0.785714285714285,0.799999999999999,0.814285714285713,0.828571428571428,
0.842857142857142,0.857142857142856,0.87142857142857,0.885714285714284,
0.899999999999999,0.914285714285713,0.928571428571427,0.942857142857141,
0.957142857142856,0.97142857142857,0.985714285714284,1.),.UNSPECIFIED.);
#114=B_SPLINE_CURVE_WITH_KNOTS('',5,(#7159,#7160,#7161,#7162,#7163,#7164,
#7165,#7166,#7167,#7168,#7169,#7170,#7171,#7172,#7173,#7174,#7175,#7176,
#7177,#7178,#7179,#7180,#7181,#7182,#7183,#7184,#7185,#7186,#7187,#7188,
#7189,#7190,#7191,#7192,#7193,#7194,#7195,#7196,#7197,#7198,#7199,#7200,
#7201,#7202,#7203,#7204,#7205,#7206,#7207,#7208,#7209,#7210,#7211,#7212,
#7213,#7214,#7215,#7216,#7217,#7218,#7219,#7220,#7221,#7222,#7223,#7224,
#7225,#7226,#7227,#7228,#7229,#7230,#7231,#7232,#7233),.UNSPECIFIED.,.F.,
 .F.,(6,1,1,1,1,1,1,1,1,1,1,1,1,1,1,1,1,1,1,1,1,1,1,1,1,1,1,1,1,1,1,1,1,
1,1,1,1,1,1,1,1,1,1,1,1,1,1,1,1,1,1,1,1,1,1,1,1,1,1,1,1,1,1,1,1,1,1,1,1,
1,6),(0.,0.0142857142857143,0.0285714285714286,0.0428571428571429,0.0571428571428571,
0.0714285714285714,0.0857142857142857,0.1,0.114285714285714,0.128571428571429,
0.142857142857143,0.157142857142857,0.171428571428571,0.185714285714286,
0.2,0.214285714285714,0.228571428571429,0.242857142857143,0.257142857142857,
0.271428571428571,0.285714285714286,0.3,0.314285714285714,0.328571428571429,
0.342857142857143,0.357142857142857,0.371428571428571,0.385714285714286,
0.4,0.414285714285714,0.428571428571429,0.442857142857143,0.457142857142857,
0.471428571428572,0.485714285714286,0.5,0.514285714285714,0.528571428571429,
0.542857142857143,0.557142857142857,0.571428571428571,0.585714285714286,
0.6,0.614285714285714,0.628571428571428,0.642857142857142,0.657142857142857,
0.671428571428571,0.685714285714285,0.699999999999999,0.714285714285714,
0.728571428571428,0.742857142857142,0.757142857142856,0.771428571428571,
0.785714285714285,0.799999999999999,0.814285714285713,0.828571428571428,
0.842857142857142,0.857142857142856,0.87142857142857,0.885714285714284,
0.899999999999999,0.914285714285713,0.928571428571427,0.942857142857141,
0.957142857142856,0.97142857142857,0.985714285714284,1.),.UNSPECIFIED.);
#115=B_SPLINE_CURVE_WITH_KNOTS('',5,(#7385,#7386,#7387,#7388,#7389,#7390,
#7391,#7392,#7393,#7394,#7395,#7396,#7397,#7398,#7399,#7400,#7401,#7402,
#7403,#7404,#7405,#7406,#7407,#7408,#7409,#7410,#7411,#7412,#7413,#7414,
#7415,#7416,#7417,#7418,#7419,#7420,#7421,#7422,#7423,#7424,#7425,#7426,
#7427,#7428,#7429,#7430,#7431,#7432,#7433,#7434,#7435,#7436,#7437,#7438,
#7439,#7440,#7441,#7442,#7443,#7444,#7445,#7446,#7447,#7448,#7449,#7450,
#7451,#7452,#7453,#7454,#7455,#7456,#7457,#7458,#7459),.UNSPECIFIED.,.F.,
 .F.,(6,1,1,1,1,1,1,1,1,1,1,1,1,1,1,1,1,1,1,1,1,1,1,1,1,1,1,1,1,1,1,1,1,
1,1,1,1,1,1,1,1,1,1,1,1,1,1,1,1,1,1,1,1,1,1,1,1,1,1,1,1,1,1,1,1,1,1,1,1,
1,6),(-1.,-0.985714285714284,-0.97142857142857,-0.957142857142856,-0.942857142857141,
-0.928571428571427,-0.914285714285713,-0.899999999999999,-0.885714285714284,
-0.87142857142857,-0.857142857142856,-0.842857142857142,-0.828571428571428,
-0.814285714285713,-0.799999999999999,-0.785714285714285,-0.771428571428571,
-0.757142857142856,-0.742857142857142,-0.728571428571428,-0.714285714285714,
-0.699999999999999,-0.685714285714285,-0.671428571428571,-0.657142857142857,
-0.642857142857142,-0.628571428571428,-0.614285714285714,-0.6,-0.585714285714286,
-0.571428571428571,-0.557142857142857,-0.542857142857143,-0.528571428571429,
-0.514285714285714,-0.5,-0.485714285714286,-0.471428571428572,-0.457142857142857,
-0.442857142857143,-0.428571428571429,-0.414285714285714,-0.4,-0.385714285714286,
-0.371428571428571,-0.357142857142857,-0.342857142857143,-0.328571428571429,
-0.314285714285714,-0.3,-0.285714285714286,-0.271428571428571,-0.257142857142857,
-0.242857142857143,-0.228571428571429,-0.214285714285714,-0.2,-0.185714285714286,
-0.171428571428571,-0.157142857142857,-0.142857142857143,-0.128571428571429,
-0.114285714285714,-0.1,-0.0857142857142857,-0.0714285714285714,-0.0571428571428571,
-0.0428571428571429,-0.0285714285714286,-0.0142857142857143,0.),
 .UNSPECIFIED.);
#116=B_SPLINE_CURVE_WITH_KNOTS('',5,(#7461,#7462,#7463,#7464,#7465,#7466,
#7467,#7468,#7469,#7470,#7471,#7472,#7473,#7474,#7475,#7476,#7477,#7478,
#7479,#7480,#7481,#7482,#7483,#7484,#7485,#7486,#7487,#7488,#7489,#7490,
#7491,#7492,#7493,#7494,#7495,#7496,#7497,#7498,#7499,#7500,#7501,#7502,
#7503,#7504,#7505,#7506,#7507,#7508,#7509,#7510,#7511,#7512,#7513,#7514,
#7515,#7516,#7517,#7518,#7519,#7520,#7521,#7522,#7523,#7524,#7525,#7526,
#7527,#7528,#7529,#7530,#7531,#7532,#7533,#7534,#7535),.UNSPECIFIED.,.F.,
 .F.,(6,1,1,1,1,1,1,1,1,1,1,1,1,1,1,1,1,1,1,1,1,1,1,1,1,1,1,1,1,1,1,1,1,
1,1,1,1,1,1,1,1,1,1,1,1,1,1,1,1,1,1,1,1,1,1,1,1,1,1,1,1,1,1,1,1,1,1,1,1,
1,6),(-1.,-0.985714285714284,-0.97142857142857,-0.957142857142856,-0.942857142857141,
-0.928571428571427,-0.914285714285713,-0.899999999999999,-0.885714285714284,
-0.87142857142857,-0.857142857142856,-0.842857142857142,-0.828571428571428,
-0.814285714285713,-0.799999999999999,-0.785714285714285,-0.771428571428571,
-0.757142857142856,-0.742857142857142,-0.728571428571428,-0.714285714285714,
-0.699999999999999,-0.685714285714285,-0.671428571428571,-0.657142857142857,
-0.642857142857142,-0.628571428571428,-0.614285714285714,-0.6,-0.585714285714286,
-0.571428571428571,-0.557142857142857,-0.542857142857143,-0.528571428571429,
-0.514285714285714,-0.5,-0.485714285714286,-0.471428571428572,-0.457142857142857,
-0.442857142857143,-0.428571428571429,-0.414285714285714,-0.4,-0.385714285714286,
-0.371428571428571,-0.357142857142857,-0.342857142857143,-0.328571428571429,
-0.314285714285714,-0.3,-0.285714285714286,-0.271428571428571,-0.257142857142857,
-0.242857142857143,-0.228571428571429,-0.214285714285714,-0.2,-0.185714285714286,
-0.171428571428571,-0.157142857142857,-0.142857142857143,-0.128571428571429,
-0.114285714285714,-0.1,-0.0857142857142857,-0.0714285714285714,-0.0571428571428571,
-0.0428571428571429,-0.0285714285714286,-0.0142857142857143,0.),
 .UNSPECIFIED.);
#117=B_SPLINE_CURVE_WITH_KNOTS('',5,(#7693,#7694,#7695,#7696,#7697,#7698,
#7699,#7700,#7701,#7702,#7703,#7704,#7705,#7706,#7707,#7708,#7709,#7710,
#7711,#7712,#7713,#7714,#7715,#7716,#7717,#7718,#7719,#7720,#7721,#7722,
#7723,#7724,#7725,#7726,#7727,#7728,#7729,#7730,#7731,#7732,#7733,#7734,
#7735,#7736,#7737,#7738,#7739,#7740,#7741,#7742,#7743,#7744,#7745,#7746,
#7747,#7748,#7749,#7750,#7751,#7752,#7753,#7754,#7755,#7756,#7757,#7758,
#7759,#7760,#7761,#7762,#7763,#7764,#7765,#7766,#7767),.UNSPECIFIED.,.F.,
 .F.,(6,1,1,1,1,1,1,1,1,1,1,1,1,1,1,1,1,1,1,1,1,1,1,1,1,1,1,1,1,1,1,1,1,
1,1,1,1,1,1,1,1,1,1,1,1,1,1,1,1,1,1,1,1,1,1,1,1,1,1,1,1,1,1,1,1,1,1,1,1,
1,6),(0.,0.0142857142857143,0.0285714285714286,0.0428571428571429,0.0571428571428571,
0.0714285714285714,0.0857142857142857,0.1,0.114285714285714,0.128571428571429,
0.142857142857143,0.157142857142857,0.171428571428571,0.185714285714286,
0.2,0.214285714285714,0.228571428571429,0.242857142857143,0.257142857142857,
0.271428571428571,0.285714285714286,0.3,0.314285714285714,0.328571428571429,
0.342857142857143,0.357142857142857,0.371428571428571,0.385714285714286,
0.4,0.414285714285714,0.428571428571429,0.442857142857143,0.457142857142857,
0.471428571428572,0.485714285714286,0.5,0.514285714285714,0.528571428571429,
0.542857142857143,0.557142857142857,0.571428571428571,0.585714285714286,
0.6,0.614285714285714,0.628571428571428,0.642857142857142,0.657142857142857,
0.671428571428571,0.685714285714285,0.699999999999999,0.714285714285714,
0.728571428571428,0.742857142857142,0.757142857142856,0.771428571428571,
0.785714285714285,0.799999999999999,0.814285714285713,0.828571428571428,
0.842857142857142,0.857142857142856,0.87142857142857,0.885714285714284,
0.899999999999999,0.914285714285713,0.928571428571427,0.942857142857141,
0.957142857142856,0.97142857142857,0.985714285714284,1.),.UNSPECIFIED.);
#118=B_SPLINE_CURVE_WITH_KNOTS('',5,(#7768,#7769,#7770,#7771,#7772,#7773,
#7774,#7775,#7776,#7777,#7778,#7779,#7780,#7781,#7782,#7783,#7784,#7785,
#7786,#7787,#7788,#7789,#7790,#7791,#7792,#7793,#7794,#7795,#7796,#7797,
#7798,#7799,#7800,#7801,#7802,#7803,#7804,#7805,#7806,#7807,#7808,#7809,
#7810,#7811,#7812,#7813,#7814,#7815,#7816,#7817,#7818,#7819,#7820,#7821,
#7822,#7823,#7824,#7825,#7826,#7827,#7828,#7829,#7830,#7831,#7832,#7833,
#7834,#7835,#7836,#7837,#7838,#7839,#7840,#7841,#7842),.UNSPECIFIED.,.F.,
 .F.,(6,1,1,1,1,1,1,1,1,1,1,1,1,1,1,1,1,1,1,1,1,1,1,1,1,1,1,1,1,1,1,1,1,
1,1,1,1,1,1,1,1,1,1,1,1,1,1,1,1,1,1,1,1,1,1,1,1,1,1,1,1,1,1,1,1,1,1,1,1,
1,6),(0.,0.0142857142857143,0.0285714285714286,0.0428571428571429,0.0571428571428571,
0.0714285714285714,0.0857142857142857,0.1,0.114285714285714,0.128571428571429,
0.142857142857143,0.157142857142857,0.171428571428571,0.185714285714286,
0.2,0.214285714285714,0.228571428571429,0.242857142857143,0.257142857142857,
0.271428571428571,0.285714285714286,0.3,0.314285714285714,0.328571428571429,
0.342857142857143,0.357142857142857,0.371428571428571,0.385714285714286,
0.4,0.414285714285714,0.428571428571429,0.442857142857143,0.457142857142857,
0.471428571428572,0.485714285714286,0.5,0.514285714285714,0.528571428571429,
0.542857142857143,0.557142857142857,0.571428571428571,0.585714285714286,
0.6,0.614285714285714,0.628571428571428,0.642857142857142,0.657142857142857,
0.671428571428571,0.685714285714285,0.699999999999999,0.714285714285714,
0.728571428571428,0.742857142857142,0.757142857142856,0.771428571428571,
0.785714285714285,0.799999999999999,0.814285714285713,0.828571428571428,
0.842857142857142,0.857142857142856,0.87142857142857,0.885714285714284,
0.899999999999999,0.914285714285713,0.928571428571427,0.942857142857141,
0.957142857142856,0.97142857142857,0.985714285714284,1.),.UNSPECIFIED.);
#119=B_SPLINE_CURVE_WITH_KNOTS('',5,(#7854,#7855,#7856,#7857,#7858,#7859,
#7860,#7861,#7862,#7863,#7864,#7865,#7866,#7867,#7868,#7869,#7870,#7871,
#7872,#7873,#7874,#7875,#7876,#7877,#7878,#7879,#7880,#7881,#7882,#7883,
#7884,#7885,#7886,#7887,#7888,#7889,#7890,#7891,#7892,#7893,#7894,#7895,
#7896,#7897,#7898,#7899,#7900,#7901,#7902,#7903,#7904,#7905,#7906,#7907,
#7908,#7909,#7910,#7911,#7912,#7913,#7914,#7915,#7916,#7917,#7918,#7919,
#7920,#7921,#7922,#7923,#7924,#7925,#7926,#7927,#7928),.UNSPECIFIED.,.F.,
 .F.,(6,1,1,1,1,1,1,1,1,1,1,1,1,1,1,1,1,1,1,1,1,1,1,1,1,1,1,1,1,1,1,1,1,
1,1,1,1,1,1,1,1,1,1,1,1,1,1,1,1,1,1,1,1,1,1,1,1,1,1,1,1,1,1,1,1,1,1,1,1,
1,6),(-1.,-0.985714285714284,-0.97142857142857,-0.957142857142856,-0.942857142857141,
-0.928571428571427,-0.914285714285713,-0.899999999999999,-0.885714285714284,
-0.87142857142857,-0.857142857142856,-0.842857142857142,-0.828571428571428,
-0.814285714285713,-0.799999999999999,-0.785714285714285,-0.771428571428571,
-0.757142857142856,-0.742857142857142,-0.728571428571428,-0.714285714285714,
-0.699999999999999,-0.685714285714285,-0.671428571428571,-0.657142857142857,
-0.642857142857142,-0.628571428571428,-0.614285714285714,-0.6,-0.585714285714286,
-0.571428571428571,-0.557142857142857,-0.542857142857143,-0.528571428571429,
-0.514285714285714,-0.5,-0.485714285714286,-0.471428571428572,-0.457142857142857,
-0.442857142857143,-0.428571428571429,-0.414285714285714,-0.4,-0.385714285714286,
-0.371428571428571,-0.357142857142857,-0.342857142857143,-0.328571428571429,
-0.314285714285714,-0.3,-0.285714285714286,-0.271428571428571,-0.257142857142857,
-0.242857142857143,-0.228571428571429,-0.214285714285714,-0.2,-0.185714285714286,
-0.171428571428571,-0.157142857142857,-0.142857142857143,-0.128571428571429,
-0.114285714285714,-0.1,-0.0857142857142857,-0.0714285714285714,-0.0571428571428571,
-0.0428571428571429,-0.0285714285714286,-0.0142857142857143,0.),
 .UNSPECIFIED.);
#120=B_SPLINE_CURVE_WITH_KNOTS('',5,(#7932,#7933,#7934,#7935,#7936,#7937,
#7938,#7939,#7940,#7941,#7942,#7943,#7944,#7945,#7946,#7947,#7948,#7949,
#7950,#7951,#7952,#7953,#7954,#7955,#7956,#7957,#7958,#7959,#7960,#7961,
#7962,#7963,#7964,#7965,#7966,#7967,#7968,#7969,#7970,#7971,#7972,#7973,
#7974,#7975,#7976,#7977,#7978,#7979,#7980,#7981,#7982,#7983,#7984,#7985,
#7986,#7987,#7988,#7989,#7990,#7991,#7992,#7993,#7994,#7995,#7996,#7997,
#7998,#7999,#8000,#8001,#8002,#8003,#8004,#8005,#8006),.UNSPECIFIED.,.F.,
 .F.,(6,1,1,1,1,1,1,1,1,1,1,1,1,1,1,1,1,1,1,1,1,1,1,1,1,1,1,1,1,1,1,1,1,
1,1,1,1,1,1,1,1,1,1,1,1,1,1,1,1,1,1,1,1,1,1,1,1,1,1,1,1,1,1,1,1,1,1,1,1,
1,6),(0.,0.0142857142857143,0.0285714285714286,0.0428571428571429,0.0571428571428571,
0.0714285714285714,0.0857142857142857,0.1,0.114285714285714,0.128571428571429,
0.142857142857143,0.157142857142857,0.171428571428571,0.185714285714286,
0.2,0.214285714285714,0.228571428571429,0.242857142857143,0.257142857142857,
0.271428571428571,0.285714285714286,0.3,0.314285714285714,0.328571428571429,
0.342857142857143,0.357142857142857,0.371428571428571,0.385714285714286,
0.4,0.414285714285714,0.428571428571429,0.442857142857143,0.457142857142857,
0.471428571428572,0.485714285714286,0.5,0.514285714285714,0.528571428571429,
0.542857142857143,0.557142857142857,0.571428571428571,0.585714285714286,
0.6,0.614285714285714,0.628571428571428,0.642857142857142,0.657142857142857,
0.671428571428571,0.685714285714285,0.699999999999999,0.714285714285714,
0.728571428571428,0.742857142857142,0.757142857142856,0.771428571428571,
0.785714285714285,0.799999999999999,0.814285714285713,0.828571428571428,
0.842857142857142,0.857142857142856,0.87142857142857,0.885714285714284,
0.899999999999999,0.914285714285713,0.928571428571427,0.942857142857141,
0.957142857142856,0.97142857142857,0.985714285714284,1.),.UNSPECIFIED.);
#121=B_SPLINE_CURVE_WITH_KNOTS('',5,(#8196,#8197,#8198,#8199,#8200,#8201,
#8202,#8203,#8204,#8205,#8206,#8207,#8208,#8209,#8210,#8211,#8212,#8213,
#8214,#8215,#8216,#8217,#8218,#8219,#8220,#8221,#8222,#8223,#8224,#8225,
#8226,#8227,#8228,#8229,#8230,#8231,#8232,#8233,#8234,#8235,#8236,#8237,
#8238,#8239,#8240,#8241,#8242,#8243,#8244,#8245,#8246,#8247,#8248,#8249,
#8250,#8251,#8252,#8253,#8254,#8255,#8256,#8257,#8258,#8259,#8260,#8261,
#8262,#8263,#8264,#8265,#8266,#8267,#8268,#8269,#8270),.UNSPECIFIED.,.F.,
 .F.,(6,1,1,1,1,1,1,1,1,1,1,1,1,1,1,1,1,1,1,1,1,1,1,1,1,1,1,1,1,1,1,1,1,
1,1,1,1,1,1,1,1,1,1,1,1,1,1,1,1,1,1,1,1,1,1,1,1,1,1,1,1,1,1,1,1,1,1,1,1,
1,6),(-1.,-0.985714285714284,-0.97142857142857,-0.957142857142856,-0.942857142857141,
-0.928571428571427,-0.914285714285713,-0.899999999999999,-0.885714285714284,
-0.87142857142857,-0.857142857142856,-0.842857142857142,-0.828571428571428,
-0.814285714285713,-0.799999999999999,-0.785714285714285,-0.771428571428571,
-0.757142857142856,-0.742857142857142,-0.728571428571428,-0.714285714285714,
-0.699999999999999,-0.685714285714285,-0.671428571428571,-0.657142857142857,
-0.642857142857142,-0.628571428571428,-0.614285714285714,-0.6,-0.585714285714286,
-0.571428571428571,-0.557142857142857,-0.542857142857143,-0.528571428571429,
-0.514285714285714,-0.5,-0.485714285714286,-0.471428571428572,-0.457142857142857,
-0.442857142857143,-0.428571428571429,-0.414285714285714,-0.4,-0.385714285714286,
-0.371428571428571,-0.357142857142857,-0.342857142857143,-0.328571428571429,
-0.314285714285714,-0.3,-0.285714285714286,-0.271428571428571,-0.257142857142857,
-0.242857142857143,-0.228571428571429,-0.214285714285714,-0.2,-0.185714285714286,
-0.171428571428571,-0.157142857142857,-0.142857142857143,-0.128571428571429,
-0.114285714285714,-0.1,-0.0857142857142857,-0.0714285714285714,-0.0571428571428571,
-0.0428571428571429,-0.0285714285714286,-0.0142857142857143,0.),
 .UNSPECIFIED.);
#122=B_SPLINE_CURVE_WITH_KNOTS('',5,(#8426,#8427,#8428,#8429,#8430,#8431,
#8432,#8433,#8434,#8435,#8436,#8437,#8438,#8439,#8440,#8441,#8442,#8443,
#8444,#8445,#8446,#8447,#8448,#8449,#8450,#8451,#8452,#8453,#8454,#8455,
#8456,#8457,#8458,#8459,#8460,#8461,#8462,#8463,#8464,#8465,#8466,#8467,
#8468,#8469,#8470,#8471,#8472,#8473,#8474,#8475,#8476,#8477,#8478,#8479,
#8480,#8481,#8482,#8483,#8484,#8485,#8486,#8487,#8488,#8489,#8490,#8491,
#8492,#8493,#8494,#8495,#8496,#8497,#8498,#8499,#8500),.UNSPECIFIED.,.F.,
 .F.,(6,1,1,1,1,1,1,1,1,1,1,1,1,1,1,1,1,1,1,1,1,1,1,1,1,1,1,1,1,1,1,1,1,
1,1,1,1,1,1,1,1,1,1,1,1,1,1,1,1,1,1,1,1,1,1,1,1,1,1,1,1,1,1,1,1,1,1,1,1,
1,6),(0.,0.0142857142857143,0.0285714285714286,0.0428571428571429,0.0571428571428571,
0.0714285714285714,0.0857142857142857,0.1,0.114285714285714,0.128571428571429,
0.142857142857143,0.157142857142857,0.171428571428571,0.185714285714286,
0.2,0.214285714285714,0.228571428571429,0.242857142857143,0.257142857142857,
0.271428571428571,0.285714285714286,0.3,0.314285714285714,0.328571428571429,
0.342857142857143,0.357142857142857,0.371428571428571,0.385714285714286,
0.4,0.414285714285714,0.428571428571429,0.442857142857143,0.457142857142857,
0.471428571428572,0.485714285714286,0.5,0.514285714285714,0.528571428571429,
0.542857142857143,0.557142857142857,0.571428571428571,0.585714285714286,
0.6,0.614285714285714,0.628571428571428,0.642857142857142,0.657142857142857,
0.671428571428571,0.685714285714285,0.699999999999999,0.714285714285714,
0.728571428571428,0.742857142857142,0.757142857142856,0.771428571428571,
0.785714285714285,0.799999999999999,0.814285714285713,0.828571428571428,
0.842857142857142,0.857142857142856,0.87142857142857,0.885714285714284,
0.899999999999999,0.914285714285713,0.928571428571427,0.942857142857141,
0.957142857142856,0.97142857142857,0.985714285714284,1.),.UNSPECIFIED.);
#123=B_SPLINE_CURVE_WITH_KNOTS('',3,(#8517,#8518,#8519,#8520,#8521,#8522,
#8523,#8524,#8525,#8526,#8527,#8528,#8529,#8530,#8531,#8532,#8533,#8534),
 .UNSPECIFIED.,.F.,.F.,(4,2,2,2,2,2,2,2,4),(0.,0.0377244205563716,0.0754488411127431,
0.113172721595804,0.150896602078865,0.188620482561925,0.226344363044986,
0.264068783601358,0.301793204157729),.UNSPECIFIED.);
#124=B_SPLINE_CURVE_WITH_KNOTS('',3,(#8535,#8536,#8537,#8538,#8539,#8540,
#8541,#8542,#8543,#8544,#8545,#8546,#8547,#8548,#8549,#8550,#8551,#8552),
 .UNSPECIFIED.,.F.,.F.,(4,2,2,2,2,2,2,2,4),(0.301793204157729,0.339517624714101,
0.377242045270472,0.414965925753533,0.452689806236594,0.490413686719655,
0.528137567202715,0.565861987759087,0.603586408315459),.UNSPECIFIED.);
#125=B_SPLINE_CURVE_WITH_KNOTS('',3,(#8568,#8569,#8570,#8571,#8572,#8573,
#8574,#8575,#8576,#8577,#8578,#8579,#8580,#8581,#8582,#8583,#8584,#8585),
 .UNSPECIFIED.,.F.,.F.,(4,2,2,2,2,2,2,2,4),(-0.302227736861757,-0.264448211272738,
-0.226668685683718,-0.188891277057298,-0.151113868430879,-0.113336459804459,
-0.0755590511780388,-0.0377795255890194,0.),.UNSPECIFIED.);
#126=B_SPLINE_CURVE_WITH_KNOTS('',3,(#8650,#8651,#8652,#8653,#8654,#8655,
#8656,#8657,#8658,#8659),.UNSPECIFIED.,.F.,.F.,(4,2,2,2,4),(-1.69587030996743,
-0.72373117051105,-0.441822634822492,-0.252830368895713,0.),
 .UNSPECIFIED.);
#127=B_SPLINE_CURVE_WITH_KNOTS('',3,(#8670,#8671,#8672,#8673,#8674,#8675,
#8676,#8677,#8678,#8679),.UNSPECIFIED.,.F.,.F.,(4,2,2,2,4),(-0.142515337540036,
-0.116550796137795,-0.0827833358078941,-0.0239794870259568,0.),
 .UNSPECIFIED.);
#128=B_SPLINE_CURVE_WITH_KNOTS('',3,(#8681,#8682,#8683,#8684,#8685,#8686,
#8687,#8688,#8689,#8690),.UNSPECIFIED.,.F.,.F.,(4,2,2,2,4),(-1.69587031141743,
-0.723731170975569,-0.441822635061051,-0.252830368989318,0.),
 .UNSPECIFIED.);
#129=B_SPLINE_CURVE_WITH_KNOTS('',3,(#8701,#8702,#8703,#8704,#8705,#8706,
#8707,#8708,#8709,#8710),.UNSPECIFIED.,.F.,.F.,(4,2,2,2,4),(-0.142515337583282,
-0.116550796158019,-0.0827833358058086,-0.0239794870257561,0.),
 .UNSPECIFIED.);
#130=B_SPLINE_CURVE_WITH_KNOTS('',3,(#8712,#8713,#8714,#8715,#8716,#8717,
#8718,#8719,#8720,#8721),.UNSPECIFIED.,.F.,.F.,(4,2,2,2,4),(-1.69587031053129,
-0.72373117069956,-0.441822634924292,-0.252830368936358,0.),
 .UNSPECIFIED.);
#131=B_SPLINE_CURVE_WITH_KNOTS('',3,(#8732,#8733,#8734,#8735,#8736,#8737,
#8738,#8739,#8740,#8741),.UNSPECIFIED.,.F.,.F.,(4,2,2,2,4),(-0.142515337525874,
-0.116550796129695,-0.0827833358062311,-0.0239794870259187,0.),
 .UNSPECIFIED.);
#132=B_SPLINE_CURVE_WITH_KNOTS('',3,(#8788,#8789,#8790,#8791,#8792,#8793,
#8794,#8795,#8796,#8797),.UNSPECIFIED.,.F.,.F.,(4,2,2,2,4),(-0.142515337540036,
-0.116550796137795,-0.0827833358078941,-0.0239794870259568,0.),
 .UNSPECIFIED.);
#133=B_SPLINE_CURVE_WITH_KNOTS('',3,(#8819,#8820,#8821,#8822,#8823,#8824,
#8825,#8826,#8827,#8828),.UNSPECIFIED.,.F.,.F.,(4,2,2,2,4),(-1.69587030996743,
-0.72373117051105,-0.441822634822492,-0.252830368895713,0.),
 .UNSPECIFIED.);
#134=B_SPLINE_CURVE_WITH_KNOTS('',3,(#8871,#8872,#8873,#8874,#8875,#8876,
#8877,#8878,#8879,#8880),.UNSPECIFIED.,.F.,.F.,(4,2,2,2,4),(-0.142515337583282,
-0.116550796158019,-0.0827833358058086,-0.0239794870257561,0.),
 .UNSPECIFIED.);
#135=B_SPLINE_CURVE_WITH_KNOTS('',3,(#8902,#8903,#8904,#8905,#8906,#8907,
#8908,#8909,#8910,#8911),.UNSPECIFIED.,.F.,.F.,(4,2,2,2,4),(-1.69587031141743,
-0.723731170975569,-0.441822635061051,-0.252830368989318,0.),
 .UNSPECIFIED.);
#136=B_SPLINE_CURVE_WITH_KNOTS('',3,(#8955,#8956,#8957,#8958,#8959,#8960,
#8961,#8962,#8963,#8964),.UNSPECIFIED.,.F.,.F.,(4,2,2,2,4),(-0.142515337525874,
-0.116550796129695,-0.0827833358062311,-0.0239794870259187,0.),
 .UNSPECIFIED.);
#137=B_SPLINE_CURVE_WITH_KNOTS('',3,(#8991,#8992,#8993,#8994,#8995,#8996,
#8997,#8998,#8999,#9000),.UNSPECIFIED.,.F.,.F.,(4,2,2,2,4),(-1.69587031053129,
-0.72373117069956,-0.441822634924292,-0.252830368936358,0.),
 .UNSPECIFIED.);
#138=B_SPLINE_CURVE_WITH_KNOTS('',3,(#9018,#9019,#9020,#9021,#9022,#9023,
#9024,#9025,#9026,#9027,#9028,#9029,#9030,#9031,#9032,#9033,#9034,#9035),
 .UNSPECIFIED.,.F.,.F.,(4,2,2,2,2,2,2,2,4),(0.,0.0377244205563716,0.0754488411127431,
0.113172721595804,0.150896602078865,0.188620482561925,0.226344363044986,
0.264068783601358,0.301793204157729),.UNSPECIFIED.);
#139=B_SPLINE_CURVE_WITH_KNOTS('',3,(#9036,#9037,#9038,#9039,#9040,#9041,
#9042,#9043,#9044,#9045,#9046,#9047,#9048,#9049,#9050,#9051,#9052,#9053),
 .UNSPECIFIED.,.F.,.F.,(4,2,2,2,2,2,2,2,4),(0.301793204157729,0.339517624714101,
0.377242045270472,0.414965925753533,0.452689806236594,0.490413686719655,
0.528137567202715,0.565861987759087,0.603586408315459),.UNSPECIFIED.);
#140=B_SPLINE_CURVE_WITH_KNOTS('',3,(#9074,#9075,#9076,#9077,#9078,#9079,
#9080,#9081,#9082,#9083,#9084,#9085,#9086,#9087,#9088,#9089,#9090,#9091),
 .UNSPECIFIED.,.F.,.F.,(4,2,2,2,2,2,2,2,4),(-0.302227736861757,-0.264448211272738,
-0.226668685683718,-0.188891277057298,-0.151113868430879,-0.113336459804459,
-0.0755590511780388,-0.0377795255890194,0.),.UNSPECIFIED.);
#141=B_SPLINE_CURVE_WITH_KNOTS('',3,(#9151,#9152,#9153,#9154,#9155,#9156,
#9157,#9158,#9159,#9160),.UNSPECIFIED.,.F.,.F.,(4,2,2,2,4),(-0.142515337525874,
-0.116550796129695,-0.0827833358062311,-0.0239794870259187,0.),
 .UNSPECIFIED.);
#142=B_SPLINE_CURVE_WITH_KNOTS('',3,(#9171,#9172,#9173,#9174,#9175,#9176,
#9177,#9178,#9179,#9180),.UNSPECIFIED.,.F.,.F.,(4,2,2,2,4),(-1.69587031053129,
-0.72373117069956,-0.441822634924292,-0.252830368936358,0.),
 .UNSPECIFIED.);
#143=B_SPLINE_CURVE_WITH_KNOTS('',3,(#9182,#9183,#9184,#9185,#9186,#9187,
#9188,#9189,#9190,#9191),.UNSPECIFIED.,.F.,.F.,(4,2,2,2,4),(-0.142515337583282,
-0.116550796158019,-0.0827833358058086,-0.0239794870257561,0.),
 .UNSPECIFIED.);
#144=B_SPLINE_CURVE_WITH_KNOTS('',3,(#9202,#9203,#9204,#9205,#9206,#9207,
#9208,#9209,#9210,#9211),.UNSPECIFIED.,.F.,.F.,(4,2,2,2,4),(-1.69587031141743,
-0.723731170975569,-0.441822635061051,-0.252830368989318,0.),
 .UNSPECIFIED.);
#145=B_SPLINE_CURVE_WITH_KNOTS('',3,(#9213,#9214,#9215,#9216,#9217,#9218,
#9219,#9220,#9221,#9222),.UNSPECIFIED.,.F.,.F.,(4,2,2,2,4),(-0.142515337540036,
-0.116550796137795,-0.0827833358078941,-0.0239794870259568,0.),
 .UNSPECIFIED.);
#146=B_SPLINE_CURVE_WITH_KNOTS('',3,(#9233,#9234,#9235,#9236,#9237,#9238,
#9239,#9240,#9241,#9242),.UNSPECIFIED.,.F.,.F.,(4,2,2,2,4),(-1.69587030996743,
-0.72373117051105,-0.441822634822492,-0.252830368895713,0.),
 .UNSPECIFIED.);
#147=B_SPLINE_CURVE_WITH_KNOTS('',3,(#9289,#9290,#9291,#9292,#9293,#9294,
#9295,#9296,#9297,#9298),.UNSPECIFIED.,.F.,.F.,(4,2,2,2,4),(-0.142515337540036,
-0.116550796137795,-0.0827833358078941,-0.0239794870259568,0.),
 .UNSPECIFIED.);
#148=B_SPLINE_CURVE_WITH_KNOTS('',3,(#9321,#9322,#9323,#9324,#9325,#9326,
#9327,#9328,#9329,#9330),.UNSPECIFIED.,.F.,.F.,(4,2,2,2,4),(-1.69587030996743,
-0.72373117051105,-0.441822634822492,-0.252830368895713,0.),
 .UNSPECIFIED.);
#149=B_SPLINE_CURVE_WITH_KNOTS('',3,(#9372,#9373,#9374,#9375,#9376,#9377,
#9378,#9379,#9380,#9381),.UNSPECIFIED.,.F.,.F.,(4,2,2,2,4),(-0.142515337583282,
-0.116550796158019,-0.0827833358058086,-0.0239794870257561,0.),
 .UNSPECIFIED.);
#150=B_SPLINE_CURVE_WITH_KNOTS('',3,(#9404,#9405,#9406,#9407,#9408,#9409,
#9410,#9411,#9412,#9413),.UNSPECIFIED.,.F.,.F.,(4,2,2,2,4),(-1.69587031141743,
-0.723731170975569,-0.441822635061051,-0.252830368989318,0.),
 .UNSPECIFIED.);
#151=B_SPLINE_CURVE_WITH_KNOTS('',3,(#9457,#9458,#9459,#9460,#9461,#9462,
#9463,#9464,#9465,#9466),.UNSPECIFIED.,.F.,.F.,(4,2,2,2,4),(-0.142515337525874,
-0.116550796129695,-0.0827833358062311,-0.0239794870259187,0.),
 .UNSPECIFIED.);
#152=B_SPLINE_CURVE_WITH_KNOTS('',3,(#9493,#9494,#9495,#9496,#9497,#9498,
#9499,#9500,#9501,#9502),.UNSPECIFIED.,.F.,.F.,(4,2,2,2,4),(-1.69587031053129,
-0.72373117069956,-0.441822634924292,-0.252830368936358,0.),
 .UNSPECIFIED.);
#153=B_SPLINE_CURVE_WITH_KNOTS('',3,(#9614,#9615,#9616,#9617,#9618,#9619,
#9620,#9621,#9622,#9623,#9624,#9625,#9626,#9627,#9628,#9629,#9630,#9631),
 .UNSPECIFIED.,.F.,.F.,(4,2,2,2,2,2,2,2,4),(0.,0.0377795255890194,0.0755590511780388,
0.113336459804459,0.151113868430879,0.188891277057298,0.226668685683718,
0.264448211272738,0.302227736861757),.UNSPECIFIED.);
#154=B_SPLINE_CURVE_WITH_KNOTS('',3,(#9644,#9645,#9646,#9647,#9648,#9649,
#9650,#9651,#9652,#9653,#9654,#9655,#9656,#9657,#9658,#9659,#9660,#9661),
 .UNSPECIFIED.,.F.,.F.,(4,2,2,2,2,2,2,2,4),(0.302227736861757,0.340007262450777,
0.377786788039796,0.415564196666216,0.453341605292636,0.491119013919056,
0.528896422545476,0.566675948134495,0.604455473723515),.UNSPECIFIED.);
#155=B_SPLINE_CURVE_WITH_KNOTS('',3,(#9682,#9683,#9684,#9685,#9686,#9687,
#9688,#9689,#9690,#9691,#9692,#9693,#9694,#9695,#9696,#9697,#9698,#9699),
 .UNSPECIFIED.,.F.,.F.,(4,2,2,2,2,2,2,2,4),(-0.302227736861757,-0.264448211272738,
-0.226668685683718,-0.188891277057298,-0.151113868430879,-0.113336459804459,
-0.0755590511780388,-0.0377795255890194,0.),.UNSPECIFIED.);
#156=B_SPLINE_CURVE_WITH_KNOTS('',3,(#9712,#9713,#9714,#9715,#9716,#9717,
#9718,#9719,#9720,#9721,#9722,#9723,#9724,#9725,#9726,#9727,#9728,#9729),
 .UNSPECIFIED.,.F.,.F.,(4,2,2,2,2,2,2,2,4),(-0.604455473723515,-0.566675948134495,
-0.528896422545476,-0.491119013919056,-0.453341605292636,-0.415564196666216,
-0.377786788039796,-0.340007262450777,-0.302227736861757),.UNSPECIFIED.);
#157=B_SPLINE_SURFACE_WITH_KNOTS('',5,1,((#4798,#4799),(#4800,#4801),(#4802,
#4803),(#4804,#4805),(#4806,#4807),(#4808,#4809),(#4810,#4811),(#4812,#4813),
(#4814,#4815),(#4816,#4817),(#4818,#4819),(#4820,#4821),(#4822,#4823),(#4824,
#4825),(#4826,#4827),(#4828,#4829),(#4830,#4831),(#4832,#4833),(#4834,#4835),
(#4836,#4837),(#4838,#4839),(#4840,#4841),(#4842,#4843),(#4844,#4845),(#4846,
#4847),(#4848,#4849),(#4850,#4851),(#4852,#4853),(#4854,#4855),(#4856,#4857),
(#4858,#4859),(#4860,#4861),(#4862,#4863),(#4864,#4865),(#4866,#4867),(#4868,
#4869),(#4870,#4871),(#4872,#4873),(#4874,#4875),(#4876,#4877),(#4878,#4879),
(#4880,#4881),(#4882,#4883),(#4884,#4885),(#4886,#4887),(#4888,#4889),(#4890,
#4891),(#4892,#4893),(#4894,#4895),(#4896,#4897),(#4898,#4899),(#4900,#4901),
(#4902,#4903),(#4904,#4905),(#4906,#4907),(#4908,#4909),(#4910,#4911),(#4912,
#4913),(#4914,#4915),(#4916,#4917),(#4918,#4919),(#4920,#4921),(#4922,#4923),
(#4924,#4925),(#4926,#4927),(#4928,#4929),(#4930,#4931),(#4932,#4933),(#4934,
#4935),(#4936,#4937),(#4938,#4939),(#4940,#4941),(#4942,#4943),(#4944,#4945),
(#4946,#4947)),.UNSPECIFIED.,.F.,.F.,.F.,(6,1,1,1,1,1,1,1,1,1,1,1,1,1,1,
1,1,1,1,1,1,1,1,1,1,1,1,1,1,1,1,1,1,1,1,1,1,1,1,1,1,1,1,1,1,1,1,1,1,1,1,
1,1,1,1,1,1,1,1,1,1,1,1,1,1,1,1,1,1,1,6),(2,2),(-1.,-0.985714285714284,
-0.97142857142857,-0.957142857142856,-0.942857142857141,-0.928571428571427,
-0.914285714285713,-0.899999999999999,-0.885714285714284,-0.87142857142857,
-0.857142857142856,-0.842857142857142,-0.828571428571428,-0.814285714285713,
-0.799999999999999,-0.785714285714285,-0.771428571428571,-0.757142857142856,
-0.742857142857142,-0.728571428571428,-0.714285714285714,-0.699999999999999,
-0.685714285714285,-0.671428571428571,-0.657142857142857,-0.642857142857142,
-0.628571428571428,-0.614285714285714,-0.6,-0.585714285714286,-0.571428571428571,
-0.557142857142857,-0.542857142857143,-0.528571428571429,-0.514285714285714,
-0.5,-0.485714285714286,-0.471428571428572,-0.457142857142857,-0.442857142857143,
-0.428571428571429,-0.414285714285714,-0.4,-0.385714285714286,-0.371428571428571,
-0.357142857142857,-0.342857142857143,-0.328571428571429,-0.314285714285714,
-0.3,-0.285714285714286,-0.271428571428571,-0.257142857142857,-0.242857142857143,
-0.228571428571429,-0.214285714285714,-0.2,-0.185714285714286,-0.171428571428571,
-0.157142857142857,-0.142857142857143,-0.128571428571429,-0.114285714285714,
-0.1,-0.0857142857142857,-0.0714285714285714,-0.0571428571428571,-0.0428571428571429,
-0.0285714285714286,-0.0142857142857143,0.),(0.,1.65),.UNSPECIFIED.);
#158=B_SPLINE_SURFACE_WITH_KNOTS('',5,1,((#5107,#5108),(#5109,#5110),(#5111,
#5112),(#5113,#5114),(#5115,#5116),(#5117,#5118),(#5119,#5120),(#5121,#5122),
(#5123,#5124),(#5125,#5126),(#5127,#5128),(#5129,#5130),(#5131,#5132),(#5133,
#5134),(#5135,#5136),(#5137,#5138),(#5139,#5140),(#5141,#5142),(#5143,#5144),
(#5145,#5146),(#5147,#5148),(#5149,#5150),(#5151,#5152),(#5153,#5154),(#5155,
#5156),(#5157,#5158),(#5159,#5160),(#5161,#5162),(#5163,#5164),(#5165,#5166),
(#5167,#5168),(#5169,#5170),(#5171,#5172),(#5173,#5174),(#5175,#5176),(#5177,
#5178),(#5179,#5180),(#5181,#5182),(#5183,#5184),(#5185,#5186),(#5187,#5188),
(#5189,#5190),(#5191,#5192),(#5193,#5194),(#5195,#5196),(#5197,#5198),(#5199,
#5200),(#5201,#5202),(#5203,#5204),(#5205,#5206),(#5207,#5208),(#5209,#5210),
(#5211,#5212),(#5213,#5214),(#5215,#5216),(#5217,#5218),(#5219,#5220),(#5221,
#5222),(#5223,#5224),(#5225,#5226),(#5227,#5228),(#5229,#5230),(#5231,#5232),
(#5233,#5234),(#5235,#5236),(#5237,#5238),(#5239,#5240),(#5241,#5242),(#5243,
#5244),(#5245,#5246),(#5247,#5248),(#5249,#5250),(#5251,#5252),(#5253,#5254),
(#5255,#5256)),.UNSPECIFIED.,.F.,.F.,.F.,(6,1,1,1,1,1,1,1,1,1,1,1,1,1,1,
1,1,1,1,1,1,1,1,1,1,1,1,1,1,1,1,1,1,1,1,1,1,1,1,1,1,1,1,1,1,1,1,1,1,1,1,
1,1,1,1,1,1,1,1,1,1,1,1,1,1,1,1,1,1,1,6),(2,2),(0.,0.0142857142857143,0.0285714285714286,
0.0428571428571429,0.0571428571428571,0.0714285714285714,0.0857142857142857,
0.1,0.114285714285714,0.128571428571429,0.142857142857143,0.157142857142857,
0.171428571428571,0.185714285714286,0.2,0.214285714285714,0.228571428571429,
0.242857142857143,0.257142857142857,0.271428571428571,0.285714285714286,
0.3,0.314285714285714,0.328571428571429,0.342857142857143,0.357142857142857,
0.371428571428571,0.385714285714286,0.4,0.414285714285714,0.428571428571429,
0.442857142857143,0.457142857142857,0.471428571428572,0.485714285714286,
0.5,0.514285714285714,0.528571428571429,0.542857142857143,0.557142857142857,
0.571428571428571,0.585714285714286,0.6,0.614285714285714,0.628571428571428,
0.642857142857142,0.657142857142857,0.671428571428571,0.685714285714285,
0.699999999999999,0.714285714285714,0.728571428571428,0.742857142857142,
0.757142857142856,0.771428571428571,0.785714285714285,0.799999999999999,
0.814285714285713,0.828571428571428,0.842857142857142,0.857142857142856,
0.87142857142857,0.885714285714284,0.899999999999999,0.914285714285713,
0.928571428571427,0.942857142857141,0.957142857142856,0.97142857142857,
0.985714285714284,1.),(0.,1.65),.UNSPECIFIED.);
#159=B_SPLINE_SURFACE_WITH_KNOTS('',5,1,((#5407,#5408),(#5409,#5410),(#5411,
#5412),(#5413,#5414),(#5415,#5416),(#5417,#5418),(#5419,#5420),(#5421,#5422),
(#5423,#5424),(#5425,#5426),(#5427,#5428),(#5429,#5430),(#5431,#5432),(#5433,
#5434),(#5435,#5436),(#5437,#5438),(#5439,#5440),(#5441,#5442),(#5443,#5444),
(#5445,#5446),(#5447,#5448),(#5449,#5450),(#5451,#5452),(#5453,#5454),(#5455,
#5456),(#5457,#5458),(#5459,#5460),(#5461,#5462),(#5463,#5464),(#5465,#5466),
(#5467,#5468),(#5469,#5470),(#5471,#5472),(#5473,#5474),(#5475,#5476),(#5477,
#5478),(#5479,#5480),(#5481,#5482),(#5483,#5484),(#5485,#5486),(#5487,#5488),
(#5489,#5490),(#5491,#5492),(#5493,#5494),(#5495,#5496),(#5497,#5498),(#5499,
#5500),(#5501,#5502),(#5503,#5504),(#5505,#5506),(#5507,#5508),(#5509,#5510),
(#5511,#5512),(#5513,#5514),(#5515,#5516),(#5517,#5518),(#5519,#5520),(#5521,
#5522),(#5523,#5524),(#5525,#5526),(#5527,#5528),(#5529,#5530),(#5531,#5532),
(#5533,#5534),(#5535,#5536),(#5537,#5538),(#5539,#5540),(#5541,#5542),(#5543,
#5544),(#5545,#5546),(#5547,#5548),(#5549,#5550),(#5551,#5552),(#5553,#5554),
(#5555,#5556)),.UNSPECIFIED.,.F.,.F.,.F.,(6,1,1,1,1,1,1,1,1,1,1,1,1,1,1,
1,1,1,1,1,1,1,1,1,1,1,1,1,1,1,1,1,1,1,1,1,1,1,1,1,1,1,1,1,1,1,1,1,1,1,1,
1,1,1,1,1,1,1,1,1,1,1,1,1,1,1,1,1,1,1,6),(2,2),(-1.,-0.985714285714284,
-0.97142857142857,-0.957142857142856,-0.942857142857141,-0.928571428571427,
-0.914285714285713,-0.899999999999999,-0.885714285714284,-0.87142857142857,
-0.857142857142856,-0.842857142857142,-0.828571428571428,-0.814285714285713,
-0.799999999999999,-0.785714285714285,-0.771428571428571,-0.757142857142856,
-0.742857142857142,-0.728571428571428,-0.714285714285714,-0.699999999999999,
-0.685714285714285,-0.671428571428571,-0.657142857142857,-0.642857142857142,
-0.628571428571428,-0.614285714285714,-0.6,-0.585714285714286,-0.571428571428571,
-0.557142857142857,-0.542857142857143,-0.528571428571429,-0.514285714285714,
-0.5,-0.485714285714286,-0.471428571428572,-0.457142857142857,-0.442857142857143,
-0.428571428571429,-0.414285714285714,-0.4,-0.385714285714286,-0.371428571428571,
-0.357142857142857,-0.342857142857143,-0.328571428571429,-0.314285714285714,
-0.3,-0.285714285714286,-0.271428571428571,-0.257142857142857,-0.242857142857143,
-0.228571428571429,-0.214285714285714,-0.2,-0.185714285714286,-0.171428571428571,
-0.157142857142857,-0.142857142857143,-0.128571428571429,-0.114285714285714,
-0.1,-0.0857142857142857,-0.0714285714285714,-0.0571428571428571,-0.0428571428571429,
-0.0285714285714286,-0.0142857142857143,0.),(0.,1.65),.UNSPECIFIED.);
#160=B_SPLINE_SURFACE_WITH_KNOTS('',5,1,((#5716,#5717),(#5718,#5719),(#5720,
#5721),(#5722,#5723),(#5724,#5725),(#5726,#5727),(#5728,#5729),(#5730,#5731),
(#5732,#5733),(#5734,#5735),(#5736,#5737),(#5738,#5739),(#5740,#5741),(#5742,
#5743),(#5744,#5745),(#5746,#5747),(#5748,#5749),(#5750,#5751),(#5752,#5753),
(#5754,#5755),(#5756,#5757),(#5758,#5759),(#5760,#5761),(#5762,#5763),(#5764,
#5765),(#5766,#5767),(#5768,#5769),(#5770,#5771),(#5772,#5773),(#5774,#5775),
(#5776,#5777),(#5778,#5779),(#5780,#5781),(#5782,#5783),(#5784,#5785),(#5786,
#5787),(#5788,#5789),(#5790,#5791),(#5792,#5793),(#5794,#5795),(#5796,#5797),
(#5798,#5799),(#5800,#5801),(#5802,#5803),(#5804,#5805),(#5806,#5807),(#5808,
#5809),(#5810,#5811),(#5812,#5813),(#5814,#5815),(#5816,#5817),(#5818,#5819),
(#5820,#5821),(#5822,#5823),(#5824,#5825),(#5826,#5827),(#5828,#5829),(#5830,
#5831),(#5832,#5833),(#5834,#5835),(#5836,#5837),(#5838,#5839),(#5840,#5841),
(#5842,#5843),(#5844,#5845),(#5846,#5847),(#5848,#5849),(#5850,#5851),(#5852,
#5853),(#5854,#5855),(#5856,#5857),(#5858,#5859),(#5860,#5861),(#5862,#5863),
(#5864,#5865)),.UNSPECIFIED.,.F.,.F.,.F.,(6,1,1,1,1,1,1,1,1,1,1,1,1,1,1,
1,1,1,1,1,1,1,1,1,1,1,1,1,1,1,1,1,1,1,1,1,1,1,1,1,1,1,1,1,1,1,1,1,1,1,1,
1,1,1,1,1,1,1,1,1,1,1,1,1,1,1,1,1,1,1,6),(2,2),(0.,0.0142857142857143,0.0285714285714286,
0.0428571428571429,0.0571428571428571,0.0714285714285714,0.0857142857142857,
0.1,0.114285714285714,0.128571428571429,0.142857142857143,0.157142857142857,
0.171428571428571,0.185714285714286,0.2,0.214285714285714,0.228571428571429,
0.242857142857143,0.257142857142857,0.271428571428571,0.285714285714286,
0.3,0.314285714285714,0.328571428571429,0.342857142857143,0.357142857142857,
0.371428571428571,0.385714285714286,0.4,0.414285714285714,0.428571428571429,
0.442857142857143,0.457142857142857,0.471428571428572,0.485714285714286,
0.5,0.514285714285714,0.528571428571429,0.542857142857143,0.557142857142857,
0.571428571428571,0.585714285714286,0.6,0.614285714285714,0.628571428571428,
0.642857142857142,0.657142857142857,0.671428571428571,0.685714285714285,
0.699999999999999,0.714285714285714,0.728571428571428,0.742857142857142,
0.757142857142856,0.771428571428571,0.785714285714285,0.799999999999999,
0.814285714285713,0.828571428571428,0.842857142857142,0.857142857142856,
0.87142857142857,0.885714285714284,0.899999999999999,0.914285714285713,
0.928571428571427,0.942857142857141,0.957142857142856,0.97142857142857,
0.985714285714284,1.),(0.,1.65),.UNSPECIFIED.);
#161=B_SPLINE_SURFACE_WITH_KNOTS('',5,1,((#6016,#6017),(#6018,#6019),(#6020,
#6021),(#6022,#6023),(#6024,#6025),(#6026,#6027),(#6028,#6029),(#6030,#6031),
(#6032,#6033),(#6034,#6035),(#6036,#6037),(#6038,#6039),(#6040,#6041),(#6042,
#6043),(#6044,#6045),(#6046,#6047),(#6048,#6049),(#6050,#6051),(#6052,#6053),
(#6054,#6055),(#6056,#6057),(#6058,#6059),(#6060,#6061),(#6062,#6063),(#6064,
#6065),(#6066,#6067),(#6068,#6069),(#6070,#6071),(#6072,#6073),(#6074,#6075),
(#6076,#6077),(#6078,#6079),(#6080,#6081),(#6082,#6083),(#6084,#6085),(#6086,
#6087),(#6088,#6089),(#6090,#6091),(#6092,#6093),(#6094,#6095),(#6096,#6097),
(#6098,#6099),(#6100,#6101),(#6102,#6103),(#6104,#6105),(#6106,#6107),(#6108,
#6109),(#6110,#6111),(#6112,#6113),(#6114,#6115),(#6116,#6117),(#6118,#6119),
(#6120,#6121),(#6122,#6123),(#6124,#6125),(#6126,#6127),(#6128,#6129),(#6130,
#6131),(#6132,#6133),(#6134,#6135),(#6136,#6137),(#6138,#6139),(#6140,#6141),
(#6142,#6143),(#6144,#6145),(#6146,#6147),(#6148,#6149),(#6150,#6151),(#6152,
#6153),(#6154,#6155),(#6156,#6157),(#6158,#6159),(#6160,#6161),(#6162,#6163),
(#6164,#6165)),.UNSPECIFIED.,.F.,.F.,.F.,(6,1,1,1,1,1,1,1,1,1,1,1,1,1,1,
1,1,1,1,1,1,1,1,1,1,1,1,1,1,1,1,1,1,1,1,1,1,1,1,1,1,1,1,1,1,1,1,1,1,1,1,
1,1,1,1,1,1,1,1,1,1,1,1,1,1,1,1,1,1,1,6),(2,2),(-1.,-0.985714285714284,
-0.97142857142857,-0.957142857142856,-0.942857142857141,-0.928571428571427,
-0.914285714285713,-0.899999999999999,-0.885714285714284,-0.87142857142857,
-0.857142857142856,-0.842857142857142,-0.828571428571428,-0.814285714285713,
-0.799999999999999,-0.785714285714285,-0.771428571428571,-0.757142857142856,
-0.742857142857142,-0.728571428571428,-0.714285714285714,-0.699999999999999,
-0.685714285714285,-0.671428571428571,-0.657142857142857,-0.642857142857142,
-0.628571428571428,-0.614285714285714,-0.6,-0.585714285714286,-0.571428571428571,
-0.557142857142857,-0.542857142857143,-0.528571428571429,-0.514285714285714,
-0.5,-0.485714285714286,-0.471428571428572,-0.457142857142857,-0.442857142857143,
-0.428571428571429,-0.414285714285714,-0.4,-0.385714285714286,-0.371428571428571,
-0.357142857142857,-0.342857142857143,-0.328571428571429,-0.314285714285714,
-0.3,-0.285714285714286,-0.271428571428571,-0.257142857142857,-0.242857142857143,
-0.228571428571429,-0.214285714285714,-0.2,-0.185714285714286,-0.171428571428571,
-0.157142857142857,-0.142857142857143,-0.128571428571429,-0.114285714285714,
-0.1,-0.0857142857142857,-0.0714285714285714,-0.0571428571428571,-0.0428571428571429,
-0.0285714285714286,-0.0142857142857143,0.),(0.,1.65),.UNSPECIFIED.);
#162=B_SPLINE_SURFACE_WITH_KNOTS('',5,1,((#6325,#6326),(#6327,#6328),(#6329,
#6330),(#6331,#6332),(#6333,#6334),(#6335,#6336),(#6337,#6338),(#6339,#6340),
(#6341,#6342),(#6343,#6344),(#6345,#6346),(#6347,#6348),(#6349,#6350),(#6351,
#6352),(#6353,#6354),(#6355,#6356),(#6357,#6358),(#6359,#6360),(#6361,#6362),
(#6363,#6364),(#6365,#6366),(#6367,#6368),(#6369,#6370),(#6371,#6372),(#6373,
#6374),(#6375,#6376),(#6377,#6378),(#6379,#6380),(#6381,#6382),(#6383,#6384),
(#6385,#6386),(#6387,#6388),(#6389,#6390),(#6391,#6392),(#6393,#6394),(#6395,
#6396),(#6397,#6398),(#6399,#6400),(#6401,#6402),(#6403,#6404),(#6405,#6406),
(#6407,#6408),(#6409,#6410),(#6411,#6412),(#6413,#6414),(#6415,#6416),(#6417,
#6418),(#6419,#6420),(#6421,#6422),(#6423,#6424),(#6425,#6426),(#6427,#6428),
(#6429,#6430),(#6431,#6432),(#6433,#6434),(#6435,#6436),(#6437,#6438),(#6439,
#6440),(#6441,#6442),(#6443,#6444),(#6445,#6446),(#6447,#6448),(#6449,#6450),
(#6451,#6452),(#6453,#6454),(#6455,#6456),(#6457,#6458),(#6459,#6460),(#6461,
#6462),(#6463,#6464),(#6465,#6466),(#6467,#6468),(#6469,#6470),(#6471,#6472),
(#6473,#6474)),.UNSPECIFIED.,.F.,.F.,.F.,(6,1,1,1,1,1,1,1,1,1,1,1,1,1,1,
1,1,1,1,1,1,1,1,1,1,1,1,1,1,1,1,1,1,1,1,1,1,1,1,1,1,1,1,1,1,1,1,1,1,1,1,
1,1,1,1,1,1,1,1,1,1,1,1,1,1,1,1,1,1,1,6),(2,2),(0.,0.0142857142857143,0.0285714285714286,
0.0428571428571429,0.0571428571428571,0.0714285714285714,0.0857142857142857,
0.1,0.114285714285714,0.128571428571429,0.142857142857143,0.157142857142857,
0.171428571428571,0.185714285714286,0.2,0.214285714285714,0.228571428571429,
0.242857142857143,0.257142857142857,0.271428571428571,0.285714285714286,
0.3,0.314285714285714,0.328571428571429,0.342857142857143,0.357142857142857,
0.371428571428571,0.385714285714286,0.4,0.414285714285714,0.428571428571429,
0.442857142857143,0.457142857142857,0.471428571428572,0.485714285714286,
0.5,0.514285714285714,0.528571428571429,0.542857142857143,0.557142857142857,
0.571428571428571,0.585714285714286,0.6,0.614285714285714,0.628571428571428,
0.642857142857142,0.657142857142857,0.671428571428571,0.685714285714285,
0.699999999999999,0.714285714285714,0.728571428571428,0.742857142857142,
0.757142857142856,0.771428571428571,0.785714285714285,0.799999999999999,
0.814285714285713,0.828571428571428,0.842857142857142,0.857142857142856,
0.87142857142857,0.885714285714284,0.899999999999999,0.914285714285713,
0.928571428571427,0.942857142857141,0.957142857142856,0.97142857142857,
0.985714285714284,1.),(0.,1.65),.UNSPECIFIED.);
#163=B_SPLINE_SURFACE_WITH_KNOTS('',5,1,((#6625,#6626),(#6627,#6628),(#6629,
#6630),(#6631,#6632),(#6633,#6634),(#6635,#6636),(#6637,#6638),(#6639,#6640),
(#6641,#6642),(#6643,#6644),(#6645,#6646),(#6647,#6648),(#6649,#6650),(#6651,
#6652),(#6653,#6654),(#6655,#6656),(#6657,#6658),(#6659,#6660),(#6661,#6662),
(#6663,#6664),(#6665,#6666),(#6667,#6668),(#6669,#6670),(#6671,#6672),(#6673,
#6674),(#6675,#6676),(#6677,#6678),(#6679,#6680),(#6681,#6682),(#6683,#6684),
(#6685,#6686),(#6687,#6688),(#6689,#6690),(#6691,#6692),(#6693,#6694),(#6695,
#6696),(#6697,#6698),(#6699,#6700),(#6701,#6702),(#6703,#6704),(#6705,#6706),
(#6707,#6708),(#6709,#6710),(#6711,#6712),(#6713,#6714),(#6715,#6716),(#6717,
#6718),(#6719,#6720),(#6721,#6722),(#6723,#6724),(#6725,#6726),(#6727,#6728),
(#6729,#6730),(#6731,#6732),(#6733,#6734),(#6735,#6736),(#6737,#6738),(#6739,
#6740),(#6741,#6742),(#6743,#6744),(#6745,#6746),(#6747,#6748),(#6749,#6750),
(#6751,#6752),(#6753,#6754),(#6755,#6756),(#6757,#6758),(#6759,#6760),(#6761,
#6762),(#6763,#6764),(#6765,#6766),(#6767,#6768),(#6769,#6770),(#6771,#6772),
(#6773,#6774)),.UNSPECIFIED.,.F.,.F.,.F.,(6,1,1,1,1,1,1,1,1,1,1,1,1,1,1,
1,1,1,1,1,1,1,1,1,1,1,1,1,1,1,1,1,1,1,1,1,1,1,1,1,1,1,1,1,1,1,1,1,1,1,1,
1,1,1,1,1,1,1,1,1,1,1,1,1,1,1,1,1,1,1,6),(2,2),(-1.,-0.985714285714284,
-0.97142857142857,-0.957142857142856,-0.942857142857141,-0.928571428571427,
-0.914285714285713,-0.899999999999999,-0.885714285714284,-0.87142857142857,
-0.857142857142856,-0.842857142857142,-0.828571428571428,-0.814285714285713,
-0.799999999999999,-0.785714285714285,-0.771428571428571,-0.757142857142856,
-0.742857142857142,-0.728571428571428,-0.714285714285714,-0.699999999999999,
-0.685714285714285,-0.671428571428571,-0.657142857142857,-0.642857142857142,
-0.628571428571428,-0.614285714285714,-0.6,-0.585714285714286,-0.571428571428571,
-0.557142857142857,-0.542857142857143,-0.528571428571429,-0.514285714285714,
-0.5,-0.485714285714286,-0.471428571428572,-0.457142857142857,-0.442857142857143,
-0.428571428571429,-0.414285714285714,-0.4,-0.385714285714286,-0.371428571428571,
-0.357142857142857,-0.342857142857143,-0.328571428571429,-0.314285714285714,
-0.3,-0.285714285714286,-0.271428571428571,-0.257142857142857,-0.242857142857143,
-0.228571428571429,-0.214285714285714,-0.2,-0.185714285714286,-0.171428571428571,
-0.157142857142857,-0.142857142857143,-0.128571428571429,-0.114285714285714,
-0.1,-0.0857142857142857,-0.0714285714285714,-0.0571428571428571,-0.0428571428571429,
-0.0285714285714286,-0.0142857142857143,0.),(0.,1.65),.UNSPECIFIED.);
#164=B_SPLINE_SURFACE_WITH_KNOTS('',5,1,((#6934,#6935),(#6936,#6937),(#6938,
#6939),(#6940,#6941),(#6942,#6943),(#6944,#6945),(#6946,#6947),(#6948,#6949),
(#6950,#6951),(#6952,#6953),(#6954,#6955),(#6956,#6957),(#6958,#6959),(#6960,
#6961),(#6962,#6963),(#6964,#6965),(#6966,#6967),(#6968,#6969),(#6970,#6971),
(#6972,#6973),(#6974,#6975),(#6976,#6977),(#6978,#6979),(#6980,#6981),(#6982,
#6983),(#6984,#6985),(#6986,#6987),(#6988,#6989),(#6990,#6991),(#6992,#6993),
(#6994,#6995),(#6996,#6997),(#6998,#6999),(#7000,#7001),(#7002,#7003),(#7004,
#7005),(#7006,#7007),(#7008,#7009),(#7010,#7011),(#7012,#7013),(#7014,#7015),
(#7016,#7017),(#7018,#7019),(#7020,#7021),(#7022,#7023),(#7024,#7025),(#7026,
#7027),(#7028,#7029),(#7030,#7031),(#7032,#7033),(#7034,#7035),(#7036,#7037),
(#7038,#7039),(#7040,#7041),(#7042,#7043),(#7044,#7045),(#7046,#7047),(#7048,
#7049),(#7050,#7051),(#7052,#7053),(#7054,#7055),(#7056,#7057),(#7058,#7059),
(#7060,#7061),(#7062,#7063),(#7064,#7065),(#7066,#7067),(#7068,#7069),(#7070,
#7071),(#7072,#7073),(#7074,#7075),(#7076,#7077),(#7078,#7079),(#7080,#7081),
(#7082,#7083)),.UNSPECIFIED.,.F.,.F.,.F.,(6,1,1,1,1,1,1,1,1,1,1,1,1,1,1,
1,1,1,1,1,1,1,1,1,1,1,1,1,1,1,1,1,1,1,1,1,1,1,1,1,1,1,1,1,1,1,1,1,1,1,1,
1,1,1,1,1,1,1,1,1,1,1,1,1,1,1,1,1,1,1,6),(2,2),(0.,0.0142857142857143,0.0285714285714286,
0.0428571428571429,0.0571428571428571,0.0714285714285714,0.0857142857142857,
0.1,0.114285714285714,0.128571428571429,0.142857142857143,0.157142857142857,
0.171428571428571,0.185714285714286,0.2,0.214285714285714,0.228571428571429,
0.242857142857143,0.257142857142857,0.271428571428571,0.285714285714286,
0.3,0.314285714285714,0.328571428571429,0.342857142857143,0.357142857142857,
0.371428571428571,0.385714285714286,0.4,0.414285714285714,0.428571428571429,
0.442857142857143,0.457142857142857,0.471428571428572,0.485714285714286,
0.5,0.514285714285714,0.528571428571429,0.542857142857143,0.557142857142857,
0.571428571428571,0.585714285714286,0.6,0.614285714285714,0.628571428571428,
0.642857142857142,0.657142857142857,0.671428571428571,0.685714285714285,
0.699999999999999,0.714285714285714,0.728571428571428,0.742857142857142,
0.757142857142856,0.771428571428571,0.785714285714285,0.799999999999999,
0.814285714285713,0.828571428571428,0.842857142857142,0.857142857142856,
0.87142857142857,0.885714285714284,0.899999999999999,0.914285714285713,
0.928571428571427,0.942857142857141,0.957142857142856,0.97142857142857,
0.985714285714284,1.),(0.,1.65),.UNSPECIFIED.);
#165=B_SPLINE_SURFACE_WITH_KNOTS('',5,1,((#7234,#7235),(#7236,#7237),(#7238,
#7239),(#7240,#7241),(#7242,#7243),(#7244,#7245),(#7246,#7247),(#7248,#7249),
(#7250,#7251),(#7252,#7253),(#7254,#7255),(#7256,#7257),(#7258,#7259),(#7260,
#7261),(#7262,#7263),(#7264,#7265),(#7266,#7267),(#7268,#7269),(#7270,#7271),
(#7272,#7273),(#7274,#7275),(#7276,#7277),(#7278,#7279),(#7280,#7281),(#7282,
#7283),(#7284,#7285),(#7286,#7287),(#7288,#7289),(#7290,#7291),(#7292,#7293),
(#7294,#7295),(#7296,#7297),(#7298,#7299),(#7300,#7301),(#7302,#7303),(#7304,
#7305),(#7306,#7307),(#7308,#7309),(#7310,#7311),(#7312,#7313),(#7314,#7315),
(#7316,#7317),(#7318,#7319),(#7320,#7321),(#7322,#7323),(#7324,#7325),(#7326,
#7327),(#7328,#7329),(#7330,#7331),(#7332,#7333),(#7334,#7335),(#7336,#7337),
(#7338,#7339),(#7340,#7341),(#7342,#7343),(#7344,#7345),(#7346,#7347),(#7348,
#7349),(#7350,#7351),(#7352,#7353),(#7354,#7355),(#7356,#7357),(#7358,#7359),
(#7360,#7361),(#7362,#7363),(#7364,#7365),(#7366,#7367),(#7368,#7369),(#7370,
#7371),(#7372,#7373),(#7374,#7375),(#7376,#7377),(#7378,#7379),(#7380,#7381),
(#7382,#7383)),.UNSPECIFIED.,.F.,.F.,.F.,(6,1,1,1,1,1,1,1,1,1,1,1,1,1,1,
1,1,1,1,1,1,1,1,1,1,1,1,1,1,1,1,1,1,1,1,1,1,1,1,1,1,1,1,1,1,1,1,1,1,1,1,
1,1,1,1,1,1,1,1,1,1,1,1,1,1,1,1,1,1,1,6),(2,2),(-1.,-0.985714285714284,
-0.97142857142857,-0.957142857142856,-0.942857142857141,-0.928571428571427,
-0.914285714285713,-0.899999999999999,-0.885714285714284,-0.87142857142857,
-0.857142857142856,-0.842857142857142,-0.828571428571428,-0.814285714285713,
-0.799999999999999,-0.785714285714285,-0.771428571428571,-0.757142857142856,
-0.742857142857142,-0.728571428571428,-0.714285714285714,-0.699999999999999,
-0.685714285714285,-0.671428571428571,-0.657142857142857,-0.642857142857142,
-0.628571428571428,-0.614285714285714,-0.6,-0.585714285714286,-0.571428571428571,
-0.557142857142857,-0.542857142857143,-0.528571428571429,-0.514285714285714,
-0.5,-0.485714285714286,-0.471428571428572,-0.457142857142857,-0.442857142857143,
-0.428571428571429,-0.414285714285714,-0.4,-0.385714285714286,-0.371428571428571,
-0.357142857142857,-0.342857142857143,-0.328571428571429,-0.314285714285714,
-0.3,-0.285714285714286,-0.271428571428571,-0.257142857142857,-0.242857142857143,
-0.228571428571429,-0.214285714285714,-0.2,-0.185714285714286,-0.171428571428571,
-0.157142857142857,-0.142857142857143,-0.128571428571429,-0.114285714285714,
-0.1,-0.0857142857142857,-0.0714285714285714,-0.0571428571428571,-0.0428571428571429,
-0.0285714285714286,-0.0142857142857143,0.),(0.,1.65),.UNSPECIFIED.);
#166=B_SPLINE_SURFACE_WITH_KNOTS('',5,1,((#7543,#7544),(#7545,#7546),(#7547,
#7548),(#7549,#7550),(#7551,#7552),(#7553,#7554),(#7555,#7556),(#7557,#7558),
(#7559,#7560),(#7561,#7562),(#7563,#7564),(#7565,#7566),(#7567,#7568),(#7569,
#7570),(#7571,#7572),(#7573,#7574),(#7575,#7576),(#7577,#7578),(#7579,#7580),
(#7581,#7582),(#7583,#7584),(#7585,#7586),(#7587,#7588),(#7589,#7590),(#7591,
#7592),(#7593,#7594),(#7595,#7596),(#7597,#7598),(#7599,#7600),(#7601,#7602),
(#7603,#7604),(#7605,#7606),(#7607,#7608),(#7609,#7610),(#7611,#7612),(#7613,
#7614),(#7615,#7616),(#7617,#7618),(#7619,#7620),(#7621,#7622),(#7623,#7624),
(#7625,#7626),(#7627,#7628),(#7629,#7630),(#7631,#7632),(#7633,#7634),(#7635,
#7636),(#7637,#7638),(#7639,#7640),(#7641,#7642),(#7643,#7644),(#7645,#7646),
(#7647,#7648),(#7649,#7650),(#7651,#7652),(#7653,#7654),(#7655,#7656),(#7657,
#7658),(#7659,#7660),(#7661,#7662),(#7663,#7664),(#7665,#7666),(#7667,#7668),
(#7669,#7670),(#7671,#7672),(#7673,#7674),(#7675,#7676),(#7677,#7678),(#7679,
#7680),(#7681,#7682),(#7683,#7684),(#7685,#7686),(#7687,#7688),(#7689,#7690),
(#7691,#7692)),.UNSPECIFIED.,.F.,.F.,.F.,(6,1,1,1,1,1,1,1,1,1,1,1,1,1,1,
1,1,1,1,1,1,1,1,1,1,1,1,1,1,1,1,1,1,1,1,1,1,1,1,1,1,1,1,1,1,1,1,1,1,1,1,
1,1,1,1,1,1,1,1,1,1,1,1,1,1,1,1,1,1,1,6),(2,2),(0.,0.0142857142857143,0.0285714285714286,
0.0428571428571429,0.0571428571428571,0.0714285714285714,0.0857142857142857,
0.1,0.114285714285714,0.128571428571429,0.142857142857143,0.157142857142857,
0.171428571428571,0.185714285714286,0.2,0.214285714285714,0.228571428571429,
0.242857142857143,0.257142857142857,0.271428571428571,0.285714285714286,
0.3,0.314285714285714,0.328571428571429,0.342857142857143,0.357142857142857,
0.371428571428571,0.385714285714286,0.4,0.414285714285714,0.428571428571429,
0.442857142857143,0.457142857142857,0.471428571428572,0.485714285714286,
0.5,0.514285714285714,0.528571428571429,0.542857142857143,0.557142857142857,
0.571428571428571,0.585714285714286,0.6,0.614285714285714,0.628571428571428,
0.642857142857142,0.657142857142857,0.671428571428571,0.685714285714285,
0.699999999999999,0.714285714285714,0.728571428571428,0.742857142857142,
0.757142857142856,0.771428571428571,0.785714285714285,0.799999999999999,
0.814285714285713,0.828571428571428,0.842857142857142,0.857142857142856,
0.87142857142857,0.885714285714284,0.899999999999999,0.914285714285713,
0.928571428571427,0.942857142857141,0.957142857142856,0.97142857142857,
0.985714285714284,1.),(0.,1.65),.UNSPECIFIED.);
#167=B_SPLINE_SURFACE_WITH_KNOTS('',5,1,((#8045,#8046),(#8047,#8048),(#8049,
#8050),(#8051,#8052),(#8053,#8054),(#8055,#8056),(#8057,#8058),(#8059,#8060),
(#8061,#8062),(#8063,#8064),(#8065,#8066),(#8067,#8068),(#8069,#8070),(#8071,
#8072),(#8073,#8074),(#8075,#8076),(#8077,#8078),(#8079,#8080),(#8081,#8082),
(#8083,#8084),(#8085,#8086),(#8087,#8088),(#8089,#8090),(#8091,#8092),(#8093,
#8094),(#8095,#8096),(#8097,#8098),(#8099,#8100),(#8101,#8102),(#8103,#8104),
(#8105,#8106),(#8107,#8108),(#8109,#8110),(#8111,#8112),(#8113,#8114),(#8115,
#8116),(#8117,#8118),(#8119,#8120),(#8121,#8122),(#8123,#8124),(#8125,#8126),
(#8127,#8128),(#8129,#8130),(#8131,#8132),(#8133,#8134),(#8135,#8136),(#8137,
#8138),(#8139,#8140),(#8141,#8142),(#8143,#8144),(#8145,#8146),(#8147,#8148),
(#8149,#8150),(#8151,#8152),(#8153,#8154),(#8155,#8156),(#8157,#8158),(#8159,
#8160),(#8161,#8162),(#8163,#8164),(#8165,#8166),(#8167,#8168),(#8169,#8170),
(#8171,#8172),(#8173,#8174),(#8175,#8176),(#8177,#8178),(#8179,#8180),(#8181,
#8182),(#8183,#8184),(#8185,#8186),(#8187,#8188),(#8189,#8190),(#8191,#8192),
(#8193,#8194)),.UNSPECIFIED.,.F.,.F.,.F.,(6,1,1,1,1,1,1,1,1,1,1,1,1,1,1,
1,1,1,1,1,1,1,1,1,1,1,1,1,1,1,1,1,1,1,1,1,1,1,1,1,1,1,1,1,1,1,1,1,1,1,1,
1,1,1,1,1,1,1,1,1,1,1,1,1,1,1,1,1,1,1,6),(2,2),(-1.,-0.985714285714284,
-0.97142857142857,-0.957142857142856,-0.942857142857141,-0.928571428571427,
-0.914285714285713,-0.899999999999999,-0.885714285714284,-0.87142857142857,
-0.857142857142856,-0.842857142857142,-0.828571428571428,-0.814285714285713,
-0.799999999999999,-0.785714285714285,-0.771428571428571,-0.757142857142856,
-0.742857142857142,-0.728571428571428,-0.714285714285714,-0.699999999999999,
-0.685714285714285,-0.671428571428571,-0.657142857142857,-0.642857142857142,
-0.628571428571428,-0.614285714285714,-0.6,-0.585714285714286,-0.571428571428571,
-0.557142857142857,-0.542857142857143,-0.528571428571429,-0.514285714285714,
-0.5,-0.485714285714286,-0.471428571428572,-0.457142857142857,-0.442857142857143,
-0.428571428571429,-0.414285714285714,-0.4,-0.385714285714286,-0.371428571428571,
-0.357142857142857,-0.342857142857143,-0.328571428571429,-0.314285714285714,
-0.3,-0.285714285714286,-0.271428571428571,-0.257142857142857,-0.242857142857143,
-0.228571428571429,-0.214285714285714,-0.2,-0.185714285714286,-0.171428571428571,
-0.157142857142857,-0.142857142857143,-0.128571428571429,-0.114285714285714,
-0.1,-0.0857142857142857,-0.0714285714285714,-0.0571428571428571,-0.0428571428571429,
-0.0285714285714286,-0.0142857142857143,0.),(0.,1.65),.UNSPECIFIED.);
#168=B_SPLINE_SURFACE_WITH_KNOTS('',5,1,((#8276,#8277),(#8278,#8279),(#8280,
#8281),(#8282,#8283),(#8284,#8285),(#8286,#8287),(#8288,#8289),(#8290,#8291),
(#8292,#8293),(#8294,#8295),(#8296,#8297),(#8298,#8299),(#8300,#8301),(#8302,
#8303),(#8304,#8305),(#8306,#8307),(#8308,#8309),(#8310,#8311),(#8312,#8313),
(#8314,#8315),(#8316,#8317),(#8318,#8319),(#8320,#8321),(#8322,#8323),(#8324,
#8325),(#8326,#8327),(#8328,#8329),(#8330,#8331),(#8332,#8333),(#8334,#8335),
(#8336,#8337),(#8338,#8339),(#8340,#8341),(#8342,#8343),(#8344,#8345),(#8346,
#8347),(#8348,#8349),(#8350,#8351),(#8352,#8353),(#8354,#8355),(#8356,#8357),
(#8358,#8359),(#8360,#8361),(#8362,#8363),(#8364,#8365),(#8366,#8367),(#8368,
#8369),(#8370,#8371),(#8372,#8373),(#8374,#8375),(#8376,#8377),(#8378,#8379),
(#8380,#8381),(#8382,#8383),(#8384,#8385),(#8386,#8387),(#8388,#8389),(#8390,
#8391),(#8392,#8393),(#8394,#8395),(#8396,#8397),(#8398,#8399),(#8400,#8401),
(#8402,#8403),(#8404,#8405),(#8406,#8407),(#8408,#8409),(#8410,#8411),(#8412,
#8413),(#8414,#8415),(#8416,#8417),(#8418,#8419),(#8420,#8421),(#8422,#8423),
(#8424,#8425)),.UNSPECIFIED.,.F.,.F.,.F.,(6,1,1,1,1,1,1,1,1,1,1,1,1,1,1,
1,1,1,1,1,1,1,1,1,1,1,1,1,1,1,1,1,1,1,1,1,1,1,1,1,1,1,1,1,1,1,1,1,1,1,1,
1,1,1,1,1,1,1,1,1,1,1,1,1,1,1,1,1,1,1,6),(2,2),(0.,0.0142857142857143,0.0285714285714286,
0.0428571428571429,0.0571428571428571,0.0714285714285714,0.0857142857142857,
0.1,0.114285714285714,0.128571428571429,0.142857142857143,0.157142857142857,
0.171428571428571,0.185714285714286,0.2,0.214285714285714,0.228571428571429,
0.242857142857143,0.257142857142857,0.271428571428571,0.285714285714286,
0.3,0.314285714285714,0.328571428571429,0.342857142857143,0.357142857142857,
0.371428571428571,0.385714285714286,0.4,0.414285714285714,0.428571428571429,
0.442857142857143,0.457142857142857,0.471428571428572,0.485714285714286,
0.5,0.514285714285714,0.528571428571429,0.542857142857143,0.557142857142857,
0.571428571428571,0.585714285714286,0.6,0.614285714285714,0.628571428571428,
0.642857142857142,0.657142857142857,0.671428571428571,0.685714285714285,
0.699999999999999,0.714285714285714,0.728571428571428,0.742857142857142,
0.757142857142856,0.771428571428571,0.785714285714285,0.799999999999999,
0.814285714285713,0.828571428571428,0.842857142857142,0.857142857142856,
0.87142857142857,0.885714285714284,0.899999999999999,0.914285714285713,
0.928571428571427,0.942857142857141,0.957142857142856,0.97142857142857,
0.985714285714284,1.),(0.,1.65),.UNSPECIFIED.);
#169=B_SPLINE_SURFACE_WITH_KNOTS('',3,1,((#8768,#8769),(#8770,#8771),(#8772,
#8773),(#8774,#8775),(#8776,#8777),(#8778,#8779),(#8780,#8781),(#8782,#8783),
(#8784,#8785),(#8786,#8787)),.UNSPECIFIED.,.F.,.F.,.F.,(4,2,2,2,4),(2,2),
(-0.142515337540036,-0.116550796137795,-0.0827833358078941,-0.0239794870259568,
0.),(0.,0.78),.UNSPECIFIED.);
#170=B_SPLINE_SURFACE_WITH_KNOTS('',3,1,((#8798,#8799),(#8800,#8801),(#8802,
#8803),(#8804,#8805),(#8806,#8807),(#8808,#8809),(#8810,#8811),(#8812,#8813),
(#8814,#8815),(#8816,#8817)),.UNSPECIFIED.,.F.,.F.,.F.,(4,2,2,2,4),(2,2),
(-1.69587030996743,-0.72373117051105,-0.441822634822492,-0.252830368895713,
0.),(0.,0.78),.UNSPECIFIED.);
#171=B_SPLINE_SURFACE_WITH_KNOTS('',3,1,((#8851,#8852),(#8853,#8854),(#8855,
#8856),(#8857,#8858),(#8859,#8860),(#8861,#8862),(#8863,#8864),(#8865,#8866),
(#8867,#8868),(#8869,#8870)),.UNSPECIFIED.,.F.,.F.,.F.,(4,2,2,2,4),(2,2),
(-0.142515337583282,-0.116550796158019,-0.0827833358058086,-0.0239794870257561,
0.),(0.,0.78),.UNSPECIFIED.);
#172=B_SPLINE_SURFACE_WITH_KNOTS('',3,1,((#8881,#8882),(#8883,#8884),(#8885,
#8886),(#8887,#8888),(#8889,#8890),(#8891,#8892),(#8893,#8894),(#8895,#8896),
(#8897,#8898),(#8899,#8900)),.UNSPECIFIED.,.F.,.F.,.F.,(4,2,2,2,4),(2,2),
(-1.69587031141743,-0.723731170975569,-0.441822635061051,-0.252830368989318,
0.),(0.,0.78),.UNSPECIFIED.);
#173=B_SPLINE_SURFACE_WITH_KNOTS('',3,1,((#8934,#8935),(#8936,#8937),(#8938,
#8939),(#8940,#8941),(#8942,#8943),(#8944,#8945),(#8946,#8947),(#8948,#8949),
(#8950,#8951),(#8952,#8953)),.UNSPECIFIED.,.F.,.F.,.F.,(4,2,2,2,4),(2,2),
(-0.142515337525874,-0.116550796129695,-0.0827833358062311,-0.0239794870259187,
0.),(0.,0.78),.UNSPECIFIED.);
#174=B_SPLINE_SURFACE_WITH_KNOTS('',3,1,((#8970,#8971),(#8972,#8973),(#8974,
#8975),(#8976,#8977),(#8978,#8979),(#8980,#8981),(#8982,#8983),(#8984,#8985),
(#8986,#8987),(#8988,#8989)),.UNSPECIFIED.,.F.,.F.,.F.,(4,2,2,2,4),(2,2),
(-1.69587031053129,-0.72373117069956,-0.441822634924292,-0.252830368936358,
0.),(0.,0.78),.UNSPECIFIED.);
#175=B_SPLINE_SURFACE_WITH_KNOTS('',3,1,((#9269,#9270),(#9271,#9272),(#9273,
#9274),(#9275,#9276),(#9277,#9278),(#9279,#9280),(#9281,#9282),(#9283,#9284),
(#9285,#9286),(#9287,#9288)),.UNSPECIFIED.,.F.,.F.,.F.,(4,2,2,2,4),(2,2),
(-0.142515337540036,-0.116550796137795,-0.0827833358078941,-0.0239794870259568,
0.),(0.,0.78),.UNSPECIFIED.);
#176=B_SPLINE_SURFACE_WITH_KNOTS('',3,1,((#9299,#9300),(#9301,#9302),(#9303,
#9304),(#9305,#9306),(#9307,#9308),(#9309,#9310),(#9311,#9312),(#9313,#9314),
(#9315,#9316),(#9317,#9318)),.UNSPECIFIED.,.F.,.F.,.F.,(4,2,2,2,4),(2,2),
(-1.69587030996743,-0.72373117051105,-0.441822634822492,-0.252830368895713,
0.),(0.,0.78),.UNSPECIFIED.);
#177=B_SPLINE_SURFACE_WITH_KNOTS('',3,1,((#9352,#9353),(#9354,#9355),(#9356,
#9357),(#9358,#9359),(#9360,#9361),(#9362,#9363),(#9364,#9365),(#9366,#9367),
(#9368,#9369),(#9370,#9371)),.UNSPECIFIED.,.F.,.F.,.F.,(4,2,2,2,4),(2,2),
(-0.142515337583282,-0.116550796158019,-0.0827833358058086,-0.0239794870257561,
0.),(0.,0.78),.UNSPECIFIED.);
#178=B_SPLINE_SURFACE_WITH_KNOTS('',3,1,((#9382,#9383),(#9384,#9385),(#9386,
#9387),(#9388,#9389),(#9390,#9391),(#9392,#9393),(#9394,#9395),(#9396,#9397),
(#9398,#9399),(#9400,#9401)),.UNSPECIFIED.,.F.,.F.,.F.,(4,2,2,2,4),(2,2),
(-1.69587031141743,-0.723731170975569,-0.441822635061051,-0.252830368989318,
0.),(0.,0.78),.UNSPECIFIED.);
#179=B_SPLINE_SURFACE_WITH_KNOTS('',3,1,((#9435,#9436),(#9437,#9438),(#9439,
#9440),(#9441,#9442),(#9443,#9444),(#9445,#9446),(#9447,#9448),(#9449,#9450),
(#9451,#9452),(#9453,#9454)),.UNSPECIFIED.,.F.,.F.,.F.,(4,2,2,2,4),(2,2),
(-0.142515337525874,-0.116550796129695,-0.0827833358062311,-0.0239794870259187,
0.),(0.,0.78),.UNSPECIFIED.);
#180=B_SPLINE_SURFACE_WITH_KNOTS('',3,1,((#9471,#9472),(#9473,#9474),(#9475,
#9476),(#9477,#9478),(#9479,#9480),(#9481,#9482),(#9483,#9484),(#9485,#9486),
(#9487,#9488),(#9489,#9490)),.UNSPECIFIED.,.F.,.F.,.F.,(4,2,2,2,4),(2,2),
(-1.69587031053129,-0.72373117069956,-0.441822634924292,-0.252830368936358,
0.),(0.,0.78),.UNSPECIFIED.);
#181=PLANE('',#3402);
#182=PLANE('',#3406);
#183=PLANE('',#3410);
#184=PLANE('',#3414);
#185=PLANE('',#3418);
#186=PLANE('',#3422);
#187=PLANE('',#3426);
#188=PLANE('',#3430);
#189=PLANE('',#3434);
#190=PLANE('',#3438);
#191=PLANE('',#3454);
#192=PLANE('',#3477);
#193=PLANE('',#3480);
#194=PLANE('',#3483);
#195=PLANE('',#3492);
#196=PLANE('',#3494);
#197=PLANE('',#3496);
#198=PLANE('',#3497);
#199=PLANE('',#3511);
#200=PLANE('',#3520);
#201=PLANE('',#3533);
#202=PLANE('',#3536);
#203=PLANE('',#3541);
#204=PLANE('',#3542);
#205=PLANE('',#3545);
#206=PLANE('',#3550);
#207=PLANE('',#3551);
#208=PLANE('',#3554);
#209=PLANE('',#3559);
#210=PLANE('',#3562);
#211=PLANE('',#3565);
#212=PLANE('',#3570);
#213=PLANE('',#3571);
#214=PLANE('',#3573);
#215=PLANE('',#3575);
#216=PLANE('',#3589);
#217=PLANE('',#3598);
#218=PLANE('',#3611);
#219=PLANE('',#3614);
#220=PLANE('',#3619);
#221=PLANE('',#3620);
#222=PLANE('',#3623);
#223=PLANE('',#3628);
#224=PLANE('',#3629);
#225=PLANE('',#3632);
#226=PLANE('',#3637);
#227=PLANE('',#3640);
#228=PLANE('',#3643);
#229=PLANE('',#3645);
#230=PLANE('',#3646);
#231=PLANE('',#3647);
#232=PLANE('',#3648);
#233=PLANE('',#3649);
#234=PLANE('',#3650);
#235=PLANE('',#3651);
#236=PLANE('',#3655);
#237=PLANE('',#3656);
#238=PLANE('',#3658);
#239=PLANE('',#3659);
#240=PLANE('',#3660);
#241=PLANE('',#3661);
#242=PLANE('',#3662);
#243=PLANE('',#3663);
#244=PLANE('',#3664);
#245=PLANE('',#3668);
#246=PLANE('',#3669);
#247=PLANE('',#3671);
#248=PLANE('',#3674);
#249=PLANE('',#3676);
#250=PLANE('',#3678);
#251=PLANE('',#3682);
#252=PLANE('',#3684);
#253=PLANE('',#3687);
#254=PLANE('',#3689);
#255=PLANE('',#3691);
#256=PLANE('',#3695);
#257=PLANE('',#3697);
#258=PLANE('',#3700);
#259=PLANE('',#3705);
#260=PLANE('',#3706);
#261=PLANE('',#3708);
#262=PLANE('',#3711);
#263=PLANE('',#3716);
#264=PLANE('',#3717);
#265=FACE_OUTER_BOUND('',#450,.T.);
#266=FACE_OUTER_BOUND('',#451,.T.);
#267=FACE_OUTER_BOUND('',#452,.T.);
#268=FACE_OUTER_BOUND('',#453,.T.);
#269=FACE_OUTER_BOUND('',#454,.T.);
#270=FACE_OUTER_BOUND('',#455,.T.);
#271=FACE_OUTER_BOUND('',#456,.T.);
#272=FACE_OUTER_BOUND('',#457,.T.);
#273=FACE_OUTER_BOUND('',#458,.T.);
#274=FACE_OUTER_BOUND('',#459,.T.);
#275=FACE_OUTER_BOUND('',#460,.T.);
#276=FACE_OUTER_BOUND('',#461,.T.);
#277=FACE_OUTER_BOUND('',#462,.T.);
#278=FACE_OUTER_BOUND('',#463,.T.);
#279=FACE_OUTER_BOUND('',#464,.T.);
#280=FACE_OUTER_BOUND('',#465,.T.);
#281=FACE_OUTER_BOUND('',#466,.T.);
#282=FACE_OUTER_BOUND('',#467,.T.);
#283=FACE_OUTER_BOUND('',#468,.T.);
#284=FACE_OUTER_BOUND('',#469,.T.);
#285=FACE_OUTER_BOUND('',#470,.T.);
#286=FACE_OUTER_BOUND('',#471,.T.);
#287=FACE_OUTER_BOUND('',#472,.T.);
#288=FACE_OUTER_BOUND('',#473,.T.);
#289=FACE_OUTER_BOUND('',#474,.T.);
#290=FACE_OUTER_BOUND('',#475,.T.);
#291=FACE_OUTER_BOUND('',#476,.T.);
#292=FACE_OUTER_BOUND('',#477,.T.);
#293=FACE_OUTER_BOUND('',#478,.T.);
#294=FACE_OUTER_BOUND('',#479,.T.);
#295=FACE_OUTER_BOUND('',#480,.T.);
#296=FACE_OUTER_BOUND('',#481,.T.);
#297=FACE_OUTER_BOUND('',#482,.T.);
#298=FACE_OUTER_BOUND('',#483,.T.);
#299=FACE_OUTER_BOUND('',#484,.T.);
#300=FACE_OUTER_BOUND('',#485,.T.);
#301=FACE_OUTER_BOUND('',#487,.T.);
#302=FACE_OUTER_BOUND('',#488,.T.);
#303=FACE_OUTER_BOUND('',#489,.T.);
#304=FACE_OUTER_BOUND('',#490,.T.);
#305=FACE_OUTER_BOUND('',#491,.T.);
#306=FACE_OUTER_BOUND('',#492,.T.);
#307=FACE_OUTER_BOUND('',#493,.T.);
#308=FACE_OUTER_BOUND('',#494,.T.);
#309=FACE_OUTER_BOUND('',#495,.T.);
#310=FACE_OUTER_BOUND('',#496,.T.);
#311=FACE_OUTER_BOUND('',#497,.T.);
#312=FACE_OUTER_BOUND('',#498,.T.);
#313=FACE_OUTER_BOUND('',#499,.T.);
#314=FACE_OUTER_BOUND('',#501,.T.);
#315=FACE_OUTER_BOUND('',#502,.T.);
#316=FACE_OUTER_BOUND('',#503,.T.);
#317=FACE_OUTER_BOUND('',#504,.T.);
#318=FACE_OUTER_BOUND('',#505,.T.);
#319=FACE_OUTER_BOUND('',#506,.T.);
#320=FACE_OUTER_BOUND('',#507,.T.);
#321=FACE_OUTER_BOUND('',#508,.T.);
#322=FACE_OUTER_BOUND('',#509,.T.);
#323=FACE_OUTER_BOUND('',#510,.T.);
#324=FACE_OUTER_BOUND('',#511,.T.);
#325=FACE_OUTER_BOUND('',#512,.T.);
#326=FACE_OUTER_BOUND('',#513,.T.);
#327=FACE_OUTER_BOUND('',#515,.T.);
#328=FACE_OUTER_BOUND('',#516,.T.);
#329=FACE_OUTER_BOUND('',#517,.T.);
#330=FACE_OUTER_BOUND('',#519,.T.);
#331=FACE_OUTER_BOUND('',#521,.T.);
#332=FACE_OUTER_BOUND('',#523,.T.);
#333=FACE_OUTER_BOUND('',#524,.T.);
#334=FACE_OUTER_BOUND('',#526,.T.);
#335=FACE_OUTER_BOUND('',#527,.T.);
#336=FACE_OUTER_BOUND('',#528,.T.);
#337=FACE_OUTER_BOUND('',#529,.T.);
#338=FACE_OUTER_BOUND('',#530,.T.);
#339=FACE_OUTER_BOUND('',#531,.T.);
#340=FACE_OUTER_BOUND('',#532,.T.);
#341=FACE_OUTER_BOUND('',#533,.T.);
#342=FACE_OUTER_BOUND('',#534,.T.);
#343=FACE_OUTER_BOUND('',#535,.T.);
#344=FACE_OUTER_BOUND('',#536,.T.);
#345=FACE_OUTER_BOUND('',#537,.T.);
#346=FACE_OUTER_BOUND('',#538,.T.);
#347=FACE_OUTER_BOUND('',#539,.T.);
#348=FACE_OUTER_BOUND('',#540,.T.);
#349=FACE_OUTER_BOUND('',#541,.T.);
#350=FACE_OUTER_BOUND('',#542,.T.);
#351=FACE_OUTER_BOUND('',#543,.T.);
#352=FACE_OUTER_BOUND('',#544,.T.);
#353=FACE_OUTER_BOUND('',#545,.T.);
#354=FACE_OUTER_BOUND('',#546,.T.);
#355=FACE_OUTER_BOUND('',#547,.T.);
#356=FACE_OUTER_BOUND('',#548,.T.);
#357=FACE_OUTER_BOUND('',#549,.T.);
#358=FACE_OUTER_BOUND('',#550,.T.);
#359=FACE_OUTER_BOUND('',#551,.T.);
#360=FACE_OUTER_BOUND('',#552,.T.);
#361=FACE_OUTER_BOUND('',#553,.T.);
#362=FACE_OUTER_BOUND('',#554,.T.);
#363=FACE_OUTER_BOUND('',#555,.T.);
#364=FACE_OUTER_BOUND('',#556,.T.);
#365=FACE_OUTER_BOUND('',#557,.T.);
#366=FACE_OUTER_BOUND('',#558,.T.);
#367=FACE_OUTER_BOUND('',#559,.T.);
#368=FACE_OUTER_BOUND('',#560,.T.);
#369=FACE_OUTER_BOUND('',#561,.T.);
#370=FACE_OUTER_BOUND('',#563,.T.);
#371=FACE_OUTER_BOUND('',#564,.T.);
#372=FACE_OUTER_BOUND('',#565,.T.);
#373=FACE_OUTER_BOUND('',#567,.T.);
#374=FACE_OUTER_BOUND('',#569,.T.);
#375=FACE_OUTER_BOUND('',#571,.T.);
#376=FACE_OUTER_BOUND('',#572,.T.);
#377=FACE_OUTER_BOUND('',#574,.T.);
#378=FACE_OUTER_BOUND('',#575,.T.);
#379=FACE_OUTER_BOUND('',#576,.T.);
#380=FACE_OUTER_BOUND('',#577,.T.);
#381=FACE_OUTER_BOUND('',#578,.T.);
#382=FACE_OUTER_BOUND('',#579,.T.);
#383=FACE_OUTER_BOUND('',#580,.T.);
#384=FACE_OUTER_BOUND('',#581,.T.);
#385=FACE_OUTER_BOUND('',#582,.T.);
#386=FACE_OUTER_BOUND('',#583,.T.);
#387=FACE_OUTER_BOUND('',#584,.T.);
#388=FACE_OUTER_BOUND('',#585,.T.);
#389=FACE_OUTER_BOUND('',#586,.T.);
#390=FACE_OUTER_BOUND('',#587,.T.);
#391=FACE_OUTER_BOUND('',#588,.T.);
#392=FACE_OUTER_BOUND('',#589,.T.);
#393=FACE_OUTER_BOUND('',#590,.T.);
#394=FACE_OUTER_BOUND('',#591,.T.);
#395=FACE_OUTER_BOUND('',#592,.T.);
#396=FACE_OUTER_BOUND('',#593,.T.);
#397=FACE_OUTER_BOUND('',#594,.T.);
#398=FACE_OUTER_BOUND('',#595,.T.);
#399=FACE_OUTER_BOUND('',#596,.T.);
#400=FACE_OUTER_BOUND('',#597,.T.);
#401=FACE_OUTER_BOUND('',#598,.T.);
#402=FACE_OUTER_BOUND('',#599,.T.);
#403=FACE_OUTER_BOUND('',#600,.T.);
#404=FACE_OUTER_BOUND('',#601,.T.);
#405=FACE_OUTER_BOUND('',#602,.T.);
#406=FACE_OUTER_BOUND('',#603,.T.);
#407=FACE_OUTER_BOUND('',#604,.T.);
#408=FACE_OUTER_BOUND('',#605,.T.);
#409=FACE_OUTER_BOUND('',#606,.T.);
#410=FACE_OUTER_BOUND('',#607,.T.);
#411=FACE_OUTER_BOUND('',#609,.T.);
#412=FACE_OUTER_BOUND('',#610,.T.);
#413=FACE_OUTER_BOUND('',#611,.T.);
#414=FACE_OUTER_BOUND('',#612,.T.);
#415=FACE_OUTER_BOUND('',#613,.T.);
#416=FACE_OUTER_BOUND('',#614,.T.);
#417=FACE_OUTER_BOUND('',#615,.T.);
#418=FACE_OUTER_BOUND('',#616,.T.);
#419=FACE_OUTER_BOUND('',#617,.T.);
#420=FACE_OUTER_BOUND('',#618,.T.);
#421=FACE_OUTER_BOUND('',#620,.T.);
#422=FACE_OUTER_BOUND('',#621,.T.);
#423=FACE_OUTER_BOUND('',#622,.T.);
#424=FACE_OUTER_BOUND('',#623,.T.);
#425=FACE_OUTER_BOUND('',#624,.T.);
#426=FACE_OUTER_BOUND('',#625,.T.);
#427=FACE_OUTER_BOUND('',#626,.T.);
#428=FACE_OUTER_BOUND('',#627,.T.);
#429=FACE_OUTER_BOUND('',#629,.T.);
#430=FACE_OUTER_BOUND('',#630,.T.);
#431=FACE_OUTER_BOUND('',#631,.T.);
#432=FACE_OUTER_BOUND('',#632,.T.);
#433=FACE_OUTER_BOUND('',#633,.T.);
#434=FACE_OUTER_BOUND('',#634,.T.);
#435=FACE_OUTER_BOUND('',#635,.T.);
#436=FACE_OUTER_BOUND('',#636,.T.);
#437=FACE_OUTER_BOUND('',#638,.T.);
#438=FACE_OUTER_BOUND('',#639,.T.);
#439=FACE_OUTER_BOUND('',#640,.T.);
#440=FACE_OUTER_BOUND('',#641,.T.);
#441=FACE_OUTER_BOUND('',#642,.T.);
#442=FACE_OUTER_BOUND('',#643,.T.);
#443=FACE_OUTER_BOUND('',#644,.T.);
#444=FACE_OUTER_BOUND('',#645,.T.);
#445=FACE_OUTER_BOUND('',#646,.T.);
#446=FACE_OUTER_BOUND('',#647,.T.);
#447=FACE_OUTER_BOUND('',#648,.T.);
#448=FACE_OUTER_BOUND('',#649,.T.);
#449=FACE_OUTER_BOUND('',#650,.T.);
#450=EDGE_LOOP('',(#2092,#2093,#2094,#2095));
#451=EDGE_LOOP('',(#2096,#2097,#2098,#2099));
#452=EDGE_LOOP('',(#2100,#2101,#2102,#2103));
#453=EDGE_LOOP('',(#2104,#2105,#2106,#2107));
#454=EDGE_LOOP('',(#2108,#2109,#2110,#2111));
#455=EDGE_LOOP('',(#2112,#2113,#2114,#2115));
#456=EDGE_LOOP('',(#2116,#2117,#2118,#2119));
#457=EDGE_LOOP('',(#2120,#2121,#2122,#2123));
#458=EDGE_LOOP('',(#2124,#2125,#2126,#2127));
#459=EDGE_LOOP('',(#2128,#2129,#2130,#2131));
#460=EDGE_LOOP('',(#2132,#2133,#2134,#2135));
#461=EDGE_LOOP('',(#2136,#2137,#2138,#2139));
#462=EDGE_LOOP('',(#2140,#2141,#2142,#2143));
#463=EDGE_LOOP('',(#2144,#2145,#2146,#2147));
#464=EDGE_LOOP('',(#2148,#2149,#2150,#2151));
#465=EDGE_LOOP('',(#2152,#2153,#2154,#2155));
#466=EDGE_LOOP('',(#2156,#2157,#2158,#2159));
#467=EDGE_LOOP('',(#2160,#2161,#2162,#2163));
#468=EDGE_LOOP('',(#2164,#2165,#2166,#2167));
#469=EDGE_LOOP('',(#2168,#2169,#2170,#2171));
#470=EDGE_LOOP('',(#2172,#2173,#2174,#2175));
#471=EDGE_LOOP('',(#2176,#2177,#2178,#2179));
#472=EDGE_LOOP('',(#2180,#2181,#2182,#2183));
#473=EDGE_LOOP('',(#2184,#2185,#2186,#2187));
#474=EDGE_LOOP('',(#2188,#2189,#2190,#2191));
#475=EDGE_LOOP('',(#2192,#2193,#2194,#2195));
#476=EDGE_LOOP('',(#2196,#2197,#2198,#2199));
#477=EDGE_LOOP('',(#2200,#2201,#2202,#2203));
#478=EDGE_LOOP('',(#2204,#2205,#2206,#2207));
#479=EDGE_LOOP('',(#2208,#2209,#2210,#2211));
#480=EDGE_LOOP('',(#2212,#2213,#2214,#2215));
#481=EDGE_LOOP('',(#2216,#2217,#2218,#2219));
#482=EDGE_LOOP('',(#2220,#2221,#2222,#2223));
#483=EDGE_LOOP('',(#2224,#2225,#2226,#2227));
#484=EDGE_LOOP('',(#2228,#2229,#2230,#2231));
#485=EDGE_LOOP('',(#2232,#2233,#2234,#2235,#2236,#2237,#2238,#2239,#2240,
#2241,#2242,#2243,#2244,#2245,#2246,#2247,#2248,#2249,#2250,#2251,#2252,
#2253,#2254,#2255,#2256,#2257,#2258,#2259,#2260,#2261,#2262,#2263,#2264,
#2265,#2266,#2267,#2268,#2269,#2270,#2271,#2272,#2273,#2274,#2275,#2276,
#2277,#2278,#2279));
#486=EDGE_LOOP('',(#2280));
#487=EDGE_LOOP('',(#2281,#2282,#2283,#2284));
#488=EDGE_LOOP('',(#2285,#2286,#2287,#2288));
#489=EDGE_LOOP('',(#2289,#2290,#2291,#2292));
#490=EDGE_LOOP('',(#2293,#2294,#2295,#2296));
#491=EDGE_LOOP('',(#2297,#2298,#2299,#2300));
#492=EDGE_LOOP('',(#2301,#2302,#2303,#2304));
#493=EDGE_LOOP('',(#2305,#2306,#2307,#2308));
#494=EDGE_LOOP('',(#2309,#2310,#2311,#2312));
#495=EDGE_LOOP('',(#2313,#2314,#2315,#2316));
#496=EDGE_LOOP('',(#2317,#2318,#2319,#2320));
#497=EDGE_LOOP('',(#2321,#2322,#2323,#2324));
#498=EDGE_LOOP('',(#2325,#2326,#2327,#2328));
#499=EDGE_LOOP('',(#2329,#2330,#2331,#2332,#2333,#2334,#2335,#2336,#2337,
#2338,#2339,#2340,#2341,#2342,#2343,#2344,#2345,#2346,#2347,#2348,#2349,
#2350,#2351,#2352,#2353,#2354,#2355,#2356,#2357,#2358,#2359,#2360,#2361,
#2362,#2363,#2364,#2365,#2366,#2367,#2368,#2369,#2370,#2371,#2372,#2373,
#2374,#2375,#2376));
#500=EDGE_LOOP('',(#2377));
#501=EDGE_LOOP('',(#2378,#2379,#2380,#2381));
#502=EDGE_LOOP('',(#2382,#2383,#2384,#2385));
#503=EDGE_LOOP('',(#2386,#2387,#2388,#2389,#2390,#2391));
#504=EDGE_LOOP('',(#2392,#2393,#2394,#2395));
#505=EDGE_LOOP('',(#2396,#2397,#2398,#2399));
#506=EDGE_LOOP('',(#2400,#2401,#2402,#2403));
#507=EDGE_LOOP('',(#2404,#2405,#2406,#2407,#2408));
#508=EDGE_LOOP('',(#2409,#2410,#2411,#2412,#2413));
#509=EDGE_LOOP('',(#2414,#2415,#2416,#2417,#2418,#2419,#2420,#2421));
#510=EDGE_LOOP('',(#2422,#2423,#2424,#2425));
#511=EDGE_LOOP('',(#2426,#2427,#2428,#2429));
#512=EDGE_LOOP('',(#2430,#2431,#2432,#2433));
#513=EDGE_LOOP('',(#2434));
#514=EDGE_LOOP('',(#2435,#2436,#2437,#2438,#2439,#2440));
#515=EDGE_LOOP('',(#2441,#2442,#2443,#2444));
#516=EDGE_LOOP('',(#2445,#2446,#2447,#2448));
#517=EDGE_LOOP('',(#2449,#2450,#2451,#2452,#2453,#2454,#2455,#2456,#2457,
#2458,#2459,#2460,#2461,#2462,#2463,#2464,#2465,#2466,#2467,#2468,#2469,
#2470,#2471,#2472));
#518=EDGE_LOOP('',(#2473));
#519=EDGE_LOOP('',(#2474,#2475,#2476,#2477));
#520=EDGE_LOOP('',(#2478,#2479));
#521=EDGE_LOOP('',(#2480));
#522=EDGE_LOOP('',(#2481,#2482,#2483,#2484,#2485));
#523=EDGE_LOOP('',(#2486,#2487,#2488,#2489));
#524=EDGE_LOOP('',(#2490));
#525=EDGE_LOOP('',(#2491));
#526=EDGE_LOOP('',(#2492,#2493,#2494,#2495));
#527=EDGE_LOOP('',(#2496,#2497,#2498,#2499));
#528=EDGE_LOOP('',(#2500,#2501,#2502,#2503));
#529=EDGE_LOOP('',(#2504,#2505,#2506,#2507,#2508));
#530=EDGE_LOOP('',(#2509,#2510,#2511,#2512,#2513));
#531=EDGE_LOOP('',(#2514,#2515,#2516,#2517));
#532=EDGE_LOOP('',(#2518,#2519,#2520,#2521));
#533=EDGE_LOOP('',(#2522,#2523,#2524,#2525,#2526,#2527,#2528,#2529));
#534=EDGE_LOOP('',(#2530,#2531,#2532,#2533));
#535=EDGE_LOOP('',(#2534,#2535,#2536,#2537));
#536=EDGE_LOOP('',(#2538,#2539,#2540,#2541));
#537=EDGE_LOOP('',(#2542,#2543,#2544,#2545,#2546));
#538=EDGE_LOOP('',(#2547,#2548,#2549,#2550,#2551));
#539=EDGE_LOOP('',(#2552,#2553,#2554,#2555));
#540=EDGE_LOOP('',(#2556,#2557,#2558,#2559));
#541=EDGE_LOOP('',(#2560,#2561,#2562,#2563,#2564,#2565,#2566,#2567));
#542=EDGE_LOOP('',(#2568,#2569,#2570,#2571));
#543=EDGE_LOOP('',(#2572,#2573,#2574,#2575));
#544=EDGE_LOOP('',(#2576,#2577,#2578,#2579));
#545=EDGE_LOOP('',(#2580,#2581,#2582,#2583,#2584));
#546=EDGE_LOOP('',(#2585,#2586,#2587,#2588));
#547=EDGE_LOOP('',(#2589,#2590,#2591,#2592,#2593));
#548=EDGE_LOOP('',(#2594,#2595,#2596,#2597));
#549=EDGE_LOOP('',(#2598,#2599,#2600,#2601));
#550=EDGE_LOOP('',(#2602,#2603,#2604,#2605,#2606,#2607,#2608,#2609));
#551=EDGE_LOOP('',(#2610,#2611,#2612,#2613,#2614,#2615));
#552=EDGE_LOOP('',(#2616,#2617,#2618,#2619));
#553=EDGE_LOOP('',(#2620,#2621,#2622,#2623));
#554=EDGE_LOOP('',(#2624,#2625,#2626,#2627,#2628));
#555=EDGE_LOOP('',(#2629,#2630,#2631,#2632));
#556=EDGE_LOOP('',(#2633,#2634,#2635,#2636,#2637));
#557=EDGE_LOOP('',(#2638,#2639,#2640,#2641,#2642,#2643,#2644,#2645));
#558=EDGE_LOOP('',(#2646,#2647,#2648,#2649));
#559=EDGE_LOOP('',(#2650,#2651,#2652,#2653));
#560=EDGE_LOOP('',(#2654,#2655,#2656,#2657));
#561=EDGE_LOOP('',(#2658));
#562=EDGE_LOOP('',(#2659,#2660,#2661,#2662,#2663,#2664));
#563=EDGE_LOOP('',(#2665,#2666,#2667,#2668));
#564=EDGE_LOOP('',(#2669,#2670,#2671,#2672));
#565=EDGE_LOOP('',(#2673,#2674,#2675,#2676,#2677,#2678,#2679,#2680,#2681,
#2682,#2683,#2684,#2685,#2686,#2687,#2688,#2689,#2690,#2691,#2692,#2693,
#2694,#2695,#2696));
#566=EDGE_LOOP('',(#2697));
#567=EDGE_LOOP('',(#2698,#2699,#2700,#2701));
#568=EDGE_LOOP('',(#2702,#2703));
#569=EDGE_LOOP('',(#2704));
#570=EDGE_LOOP('',(#2705,#2706,#2707,#2708,#2709));
#571=EDGE_LOOP('',(#2710,#2711,#2712,#2713));
#572=EDGE_LOOP('',(#2714));
#573=EDGE_LOOP('',(#2715));
#574=EDGE_LOOP('',(#2716,#2717,#2718,#2719));
#575=EDGE_LOOP('',(#2720,#2721,#2722,#2723));
#576=EDGE_LOOP('',(#2724,#2725,#2726,#2727));
#577=EDGE_LOOP('',(#2728,#2729,#2730,#2731,#2732));
#578=EDGE_LOOP('',(#2733,#2734,#2735,#2736,#2737));
#579=EDGE_LOOP('',(#2738,#2739,#2740,#2741));
#580=EDGE_LOOP('',(#2742,#2743,#2744,#2745));
#581=EDGE_LOOP('',(#2746,#2747,#2748,#2749,#2750,#2751,#2752,#2753));
#582=EDGE_LOOP('',(#2754,#2755,#2756,#2757));
#583=EDGE_LOOP('',(#2758,#2759,#2760,#2761));
#584=EDGE_LOOP('',(#2762,#2763,#2764,#2765));
#585=EDGE_LOOP('',(#2766,#2767,#2768,#2769,#2770));
#586=EDGE_LOOP('',(#2771,#2772,#2773,#2774,#2775));
#587=EDGE_LOOP('',(#2776,#2777,#2778,#2779));
#588=EDGE_LOOP('',(#2780,#2781,#2782,#2783));
#589=EDGE_LOOP('',(#2784,#2785,#2786,#2787,#2788,#2789,#2790,#2791));
#590=EDGE_LOOP('',(#2792,#2793,#2794,#2795));
#591=EDGE_LOOP('',(#2796,#2797,#2798,#2799));
#592=EDGE_LOOP('',(#2800,#2801,#2802,#2803));
#593=EDGE_LOOP('',(#2804,#2805,#2806,#2807,#2808));
#594=EDGE_LOOP('',(#2809,#2810,#2811,#2812));
#595=EDGE_LOOP('',(#2813,#2814,#2815,#2816,#2817));
#596=EDGE_LOOP('',(#2818,#2819,#2820,#2821));
#597=EDGE_LOOP('',(#2822,#2823,#2824,#2825));
#598=EDGE_LOOP('',(#2826,#2827,#2828,#2829,#2830,#2831,#2832,#2833));
#599=EDGE_LOOP('',(#2834,#2835,#2836,#2837));
#600=EDGE_LOOP('',(#2838,#2839,#2840,#2841));
#601=EDGE_LOOP('',(#2842,#2843,#2844,#2845));
#602=EDGE_LOOP('',(#2846,#2847,#2848,#2849));
#603=EDGE_LOOP('',(#2850,#2851,#2852,#2853));
#604=EDGE_LOOP('',(#2854,#2855,#2856,#2857));
#605=EDGE_LOOP('',(#2858,#2859,#2860,#2861,#2862,#2863));
#606=EDGE_LOOP('',(#2864,#2865,#2866,#2867));
#607=EDGE_LOOP('',(#2868));
#608=EDGE_LOOP('',(#2869,#2870,#2871,#2872,#2873,#2874));
#609=EDGE_LOOP('',(#2875));
#610=EDGE_LOOP('',(#2876,#2877,#2878,#2879));
#611=EDGE_LOOP('',(#2880,#2881,#2882,#2883));
#612=EDGE_LOOP('',(#2884,#2885,#2886,#2887));
#613=EDGE_LOOP('',(#2888,#2889,#2890,#2891));
#614=EDGE_LOOP('',(#2892,#2893,#2894,#2895));
#615=EDGE_LOOP('',(#2896,#2897,#2898,#2899));
#616=EDGE_LOOP('',(#2900,#2901,#2902,#2903,#2904,#2905));
#617=EDGE_LOOP('',(#2906,#2907,#2908,#2909));
#618=EDGE_LOOP('',(#2910));
#619=EDGE_LOOP('',(#2911,#2912,#2913,#2914,#2915,#2916));
#620=EDGE_LOOP('',(#2917));
#621=EDGE_LOOP('',(#2918,#2919,#2920,#2921));
#622=EDGE_LOOP('',(#2922,#2923,#2924,#2925));
#623=EDGE_LOOP('',(#2926,#2927,#2928,#2929));
#624=EDGE_LOOP('',(#2930,#2931,#2932,#2933));
#625=EDGE_LOOP('',(#2934,#2935,#2936,#2937));
#626=EDGE_LOOP('',(#2938));
#627=EDGE_LOOP('',(#2939,#2940,#2941,#2942));
#628=EDGE_LOOP('',(#2943,#2944,#2945,#2946));
#629=EDGE_LOOP('',(#2947));
#630=EDGE_LOOP('',(#2948,#2949,#2950,#2951));
#631=EDGE_LOOP('',(#2952,#2953,#2954,#2955));
#632=EDGE_LOOP('',(#2956,#2957,#2958,#2959));
#633=EDGE_LOOP('',(#2960,#2961,#2962,#2963));
#634=EDGE_LOOP('',(#2964,#2965,#2966,#2967));
#635=EDGE_LOOP('',(#2968));
#636=EDGE_LOOP('',(#2969,#2970,#2971,#2972));
#637=EDGE_LOOP('',(#2973,#2974,#2975,#2976));
#638=EDGE_LOOP('',(#2977));
#639=EDGE_LOOP('',(#2978,#2979,#2980,#2981));
#640=EDGE_LOOP('',(#2982,#2983,#2984,#2985));
#641=EDGE_LOOP('',(#2986,#2987,#2988,#2989));
#642=EDGE_LOOP('',(#2990,#2991,#2992,#2993));
#643=EDGE_LOOP('',(#2994,#2995,#2996,#2997));
#644=EDGE_LOOP('',(#2998,#2999,#3000,#3001));
#645=EDGE_LOOP('',(#3002,#3003,#3004,#3005));
#646=EDGE_LOOP('',(#3006,#3007,#3008,#3009));
#647=EDGE_LOOP('',(#3010,#3011,#3012,#3013));
#648=EDGE_LOOP('',(#3014,#3015,#3016,#3017));
#649=EDGE_LOOP('',(#3018,#3019,#3020,#3021));
#650=EDGE_LOOP('',(#3022,#3023,#3024,#3025));
#651=LINE('',#4653,#910);
#652=LINE('',#4656,#911);
#653=LINE('',#4659,#912);
#654=LINE('',#4661,#913);
#655=LINE('',#4662,#914);
#656=LINE('',#4668,#915);
#657=LINE('',#4671,#916);
#658=LINE('',#4674,#917);
#659=LINE('',#4676,#918);
#660=LINE('',#4677,#919);
#661=LINE('',#4683,#920);
#662=LINE('',#4686,#921);
#663=LINE('',#4689,#922);
#664=LINE('',#4691,#923);
#665=LINE('',#4692,#924);
#666=LINE('',#4698,#925);
#667=LINE('',#4701,#926);
#668=LINE('',#4704,#927);
#669=LINE('',#4706,#928);
#670=LINE('',#4707,#929);
#671=LINE('',#4713,#930);
#672=LINE('',#4716,#931);
#673=LINE('',#4719,#932);
#674=LINE('',#4721,#933);
#675=LINE('',#4722,#934);
#676=LINE('',#4728,#935);
#677=LINE('',#4731,#936);
#678=LINE('',#4734,#937);
#679=LINE('',#4736,#938);
#680=LINE('',#4737,#939);
#681=LINE('',#4743,#940);
#682=LINE('',#4746,#941);
#683=LINE('',#4749,#942);
#684=LINE('',#4751,#943);
#685=LINE('',#4752,#944);
#686=LINE('',#4758,#945);
#687=LINE('',#4761,#946);
#688=LINE('',#4764,#947);
#689=LINE('',#4766,#948);
#690=LINE('',#4767,#949);
#691=LINE('',#4773,#950);
#692=LINE('',#4776,#951);
#693=LINE('',#4779,#952);
#694=LINE('',#4781,#953);
#695=LINE('',#4782,#954);
#696=LINE('',#4788,#955);
#697=LINE('',#4791,#956);
#698=LINE('',#4794,#957);
#699=LINE('',#4796,#958);
#700=LINE('',#4797,#959);
#701=LINE('',#5100,#960);
#702=LINE('',#5106,#961);
#703=LINE('',#5709,#962);
#704=LINE('',#5715,#963);
#705=LINE('',#6318,#964);
#706=LINE('',#6324,#965);
#707=LINE('',#6927,#966);
#708=LINE('',#6933,#967);
#709=LINE('',#7536,#968);
#710=LINE('',#7542,#969);
#711=LINE('',#7852,#970);
#712=LINE('',#8008,#971);
#713=LINE('',#8018,#972);
#714=LINE('',#8030,#973);
#715=LINE('',#8033,#974);
#716=LINE('',#8034,#975);
#717=LINE('',#8037,#976);
#718=LINE('',#8040,#977);
#719=LINE('',#8043,#978);
#720=LINE('',#8044,#979);
#721=LINE('',#8271,#980);
#722=LINE('',#8275,#981);
#723=LINE('',#8506,#982);
#724=LINE('',#8515,#983);
#725=LINE('',#8555,#984);
#726=LINE('',#8558,#985);
#727=LINE('',#8561,#986);
#728=LINE('',#8563,#987);
#729=LINE('',#8564,#988);
#730=LINE('',#8586,#989);
#731=LINE('',#8587,#990);
#732=LINE('',#8590,#991);
#733=LINE('',#8591,#992);
#734=LINE('',#8594,#993);
#735=LINE('',#8595,#994);
#736=LINE('',#8600,#995);
#737=LINE('',#8606,#996);
#738=LINE('',#8610,#997);
#739=LINE('',#8615,#998);
#740=LINE('',#8619,#999);
#741=LINE('',#8624,#1000);
#742=LINE('',#8628,#1001);
#743=LINE('',#8638,#1002);
#744=LINE('',#8641,#1003);
#745=LINE('',#8644,#1004);
#746=LINE('',#8647,#1005);
#747=LINE('',#8661,#1006);
#748=LINE('',#8669,#1007);
#749=LINE('',#8692,#1008);
#750=LINE('',#8700,#1009);
#751=LINE('',#8723,#1010);
#752=LINE('',#8731,#1011);
#753=LINE('',#8746,#1012);
#754=LINE('',#8752,#1013);
#755=LINE('',#8756,#1014);
#756=LINE('',#8759,#1015);
#757=LINE('',#8763,#1016);
#758=LINE('',#8766,#1017);
#759=LINE('',#8767,#1018);
#760=LINE('',#8829,#1019);
#761=LINE('',#8832,#1020);
#762=LINE('',#8833,#1021);
#763=LINE('',#8839,#1022);
#764=LINE('',#8842,#1023);
#765=LINE('',#8846,#1024);
#766=LINE('',#8849,#1025);
#767=LINE('',#8850,#1026);
#768=LINE('',#8912,#1027);
#769=LINE('',#8915,#1028);
#770=LINE('',#8916,#1029);
#771=LINE('',#8922,#1030);
#772=LINE('',#8925,#1031);
#773=LINE('',#8929,#1032);
#774=LINE('',#8932,#1033);
#775=LINE('',#8933,#1034);
#776=LINE('',#8965,#1035);
#777=LINE('',#8969,#1036);
#778=LINE('',#9001,#1037);
#779=LINE('',#9004,#1038);
#780=LINE('',#9005,#1039);
#781=LINE('',#9016,#1040);
#782=LINE('',#9056,#1041);
#783=LINE('',#9058,#1042);
#784=LINE('',#9059,#1043);
#785=LINE('',#9062,#1044);
#786=LINE('',#9065,#1045);
#787=LINE('',#9068,#1046);
#788=LINE('',#9070,#1047);
#789=LINE('',#9071,#1048);
#790=LINE('',#9092,#1049);
#791=LINE('',#9095,#1050);
#792=LINE('',#9096,#1051);
#793=LINE('',#9101,#1052);
#794=LINE('',#9107,#1053);
#795=LINE('',#9111,#1054);
#796=LINE('',#9116,#1055);
#797=LINE('',#9120,#1056);
#798=LINE('',#9125,#1057);
#799=LINE('',#9129,#1058);
#800=LINE('',#9139,#1059);
#801=LINE('',#9142,#1060);
#802=LINE('',#9145,#1061);
#803=LINE('',#9148,#1062);
#804=LINE('',#9162,#1063);
#805=LINE('',#9170,#1064);
#806=LINE('',#9193,#1065);
#807=LINE('',#9201,#1066);
#808=LINE('',#9224,#1067);
#809=LINE('',#9232,#1068);
#810=LINE('',#9247,#1069);
#811=LINE('',#9252,#1070);
#812=LINE('',#9257,#1071);
#813=LINE('',#9260,#1072);
#814=LINE('',#9263,#1073);
#815=LINE('',#9267,#1074);
#816=LINE('',#9268,#1075);
#817=LINE('',#9320,#1076);
#818=LINE('',#9333,#1077);
#819=LINE('',#9334,#1078);
#820=LINE('',#9340,#1079);
#821=LINE('',#9343,#1080);
#822=LINE('',#9346,#1081);
#823=LINE('',#9350,#1082);
#824=LINE('',#9351,#1083);
#825=LINE('',#9403,#1084);
#826=LINE('',#9416,#1085);
#827=LINE('',#9417,#1086);
#828=LINE('',#9423,#1087);
#829=LINE('',#9426,#1088);
#830=LINE('',#9429,#1089);
#831=LINE('',#9433,#1090);
#832=LINE('',#9434,#1091);
#833=LINE('',#9456,#1092);
#834=LINE('',#9469,#1093);
#835=LINE('',#9492,#1094);
#836=LINE('',#9505,#1095);
#837=LINE('',#9506,#1096);
#838=LINE('',#9514,#1097);
#839=LINE('',#9516,#1098);
#840=LINE('',#9518,#1099);
#841=LINE('',#9519,#1100);
#842=LINE('',#9522,#1101);
#843=LINE('',#9524,#1102);
#844=LINE('',#9525,#1103);
#845=LINE('',#9528,#1104);
#846=LINE('',#9530,#1105);
#847=LINE('',#9531,#1106);
#848=LINE('',#9534,#1107);
#849=LINE('',#9536,#1108);
#850=LINE('',#9537,#1109);
#851=LINE('',#9540,#1110);
#852=LINE('',#9542,#1111);
#853=LINE('',#9543,#1112);
#854=LINE('',#9545,#1113);
#855=LINE('',#9546,#1114);
#856=LINE('',#9552,#1115);
#857=LINE('',#9560,#1116);
#858=LINE('',#9562,#1117);
#859=LINE('',#9564,#1118);
#860=LINE('',#9565,#1119);
#861=LINE('',#9568,#1120);
#862=LINE('',#9570,#1121);
#863=LINE('',#9571,#1122);
#864=LINE('',#9574,#1123);
#865=LINE('',#9576,#1124);
#866=LINE('',#9577,#1125);
#867=LINE('',#9580,#1126);
#868=LINE('',#9582,#1127);
#869=LINE('',#9583,#1128);
#870=LINE('',#9586,#1129);
#871=LINE('',#9588,#1130);
#872=LINE('',#9589,#1131);
#873=LINE('',#9591,#1132);
#874=LINE('',#9592,#1133);
#875=LINE('',#9598,#1134);
#876=LINE('',#9606,#1135);
#877=LINE('',#9608,#1136);
#878=LINE('',#9610,#1137);
#879=LINE('',#9611,#1138);
#880=LINE('',#9634,#1139);
#881=LINE('',#9638,#1140);
#882=LINE('',#9641,#1141);
#883=LINE('',#9642,#1142);
#884=LINE('',#9668,#1143);
#885=LINE('',#9674,#1144);
#886=LINE('',#9676,#1145);
#887=LINE('',#9678,#1146);
#888=LINE('',#9679,#1147);
#889=LINE('',#9701,#1148);
#890=LINE('',#9705,#1149);
#891=LINE('',#9709,#1150);
#892=LINE('',#9710,#1151);
#893=LINE('',#9735,#1152);
#894=LINE('',#9744,#1153);
#895=LINE('',#9747,#1154);
#896=LINE('',#9750,#1155);
#897=LINE('',#9752,#1156);
#898=LINE('',#9753,#1157);
#899=LINE('',#9757,#1158);
#900=LINE('',#9760,#1159);
#901=LINE('',#9763,#1160);
#902=LINE('',#9771,#1161);
#903=LINE('',#9774,#1162);
#904=LINE('',#9777,#1163);
#905=LINE('',#9779,#1164);
#906=LINE('',#9780,#1165);
#907=LINE('',#9783,#1166);
#908=LINE('',#9788,#1167);
#909=LINE('',#9790,#1168);
#910=VECTOR('',#3735,10.);
#911=VECTOR('',#3738,10.);
#912=VECTOR('',#3741,10.);
#913=VECTOR('',#3742,10.);
#914=VECTOR('',#3743,10.);
#915=VECTOR('',#3748,10.);
#916=VECTOR('',#3751,10.);
#917=VECTOR('',#3754,10.);
#918=VECTOR('',#3755,10.);
#919=VECTOR('',#3756,10.);
#920=VECTOR('',#3761,10.);
#921=VECTOR('',#3764,10.);
#922=VECTOR('',#3767,10.);
#923=VECTOR('',#3768,10.);
#924=VECTOR('',#3769,10.);
#925=VECTOR('',#3774,10.);
#926=VECTOR('',#3777,10.);
#927=VECTOR('',#3780,10.);
#928=VECTOR('',#3781,10.);
#929=VECTOR('',#3782,10.);
#930=VECTOR('',#3787,10.);
#931=VECTOR('',#3790,10.);
#932=VECTOR('',#3793,10.);
#933=VECTOR('',#3794,10.);
#934=VECTOR('',#3795,10.);
#935=VECTOR('',#3800,10.);
#936=VECTOR('',#3803,10.);
#937=VECTOR('',#3806,10.);
#938=VECTOR('',#3807,10.);
#939=VECTOR('',#3808,10.);
#940=VECTOR('',#3813,10.);
#941=VECTOR('',#3816,10.);
#942=VECTOR('',#3819,10.);
#943=VECTOR('',#3820,10.);
#944=VECTOR('',#3821,10.);
#945=VECTOR('',#3826,10.);
#946=VECTOR('',#3829,10.);
#947=VECTOR('',#3832,10.);
#948=VECTOR('',#3833,10.);
#949=VECTOR('',#3834,10.);
#950=VECTOR('',#3839,10.);
#951=VECTOR('',#3842,10.);
#952=VECTOR('',#3845,10.);
#953=VECTOR('',#3846,10.);
#954=VECTOR('',#3847,10.);
#955=VECTOR('',#3852,10.);
#956=VECTOR('',#3855,10.);
#957=VECTOR('',#3858,10.);
#958=VECTOR('',#3859,10.);
#959=VECTOR('',#3860,10.);
#960=VECTOR('',#3861,10.);
#961=VECTOR('',#3868,10.);
#962=VECTOR('',#3869,10.);
#963=VECTOR('',#3876,10.);
#964=VECTOR('',#3877,10.);
#965=VECTOR('',#3884,10.);
#966=VECTOR('',#3885,10.);
#967=VECTOR('',#3892,10.);
#968=VECTOR('',#3893,10.);
#969=VECTOR('',#3900,10.);
#970=VECTOR('',#3913,10.);
#971=VECTOR('',#3916,10.);
#972=VECTOR('',#3929,10.);
#973=VECTOR('',#3950,10.);
#974=VECTOR('',#3953,10.);
#975=VECTOR('',#3954,10.);
#976=VECTOR('',#3957,10.);
#977=VECTOR('',#3960,10.);
#978=VECTOR('',#3963,10.);
#979=VECTOR('',#3964,10.);
#980=VECTOR('',#3965,10.);
#981=VECTOR('',#3970,10.);
#982=VECTOR('',#3979,5.);
#983=VECTOR('',#3990,1.);
#984=VECTOR('',#3993,10.);
#985=VECTOR('',#3996,10.);
#986=VECTOR('',#3999,10.);
#987=VECTOR('',#4000,10.);
#988=VECTOR('',#4001,10.);
#989=VECTOR('',#4004,10.);
#990=VECTOR('',#4005,10.);
#991=VECTOR('',#4008,10.);
#992=VECTOR('',#4009,10.);
#993=VECTOR('',#4012,10.);
#994=VECTOR('',#4013,10.);
#995=VECTOR('',#4018,5.);
#996=VECTOR('',#4025,10.);
#997=VECTOR('',#4028,10.);
#998=VECTOR('',#4033,10.);
#999=VECTOR('',#4036,10.);
#1000=VECTOR('',#4041,10.);
#1001=VECTOR('',#4044,10.);
#1002=VECTOR('',#4059,10.);
#1003=VECTOR('',#4062,10.);
#1004=VECTOR('',#4065,10.);
#1005=VECTOR('',#4068,10.);
#1006=VECTOR('',#4071,10.);
#1007=VECTOR('',#4078,10.);
#1008=VECTOR('',#4079,10.);
#1009=VECTOR('',#4086,10.);
#1010=VECTOR('',#4087,10.);
#1011=VECTOR('',#4094,10.);
#1012=VECTOR('',#4099,7.);
#1013=VECTOR('',#4108,13.5);
#1014=VECTOR('',#4113,10.);
#1015=VECTOR('',#4116,10.);
#1016=VECTOR('',#4121,10.);
#1017=VECTOR('',#4124,10.);
#1018=VECTOR('',#4125,10.);
#1019=VECTOR('',#4126,10.);
#1020=VECTOR('',#4129,10.);
#1021=VECTOR('',#4130,10.);
#1022=VECTOR('',#4139,10.);
#1023=VECTOR('',#4142,10.);
#1024=VECTOR('',#4147,10.);
#1025=VECTOR('',#4150,10.);
#1026=VECTOR('',#4151,10.);
#1027=VECTOR('',#4152,10.);
#1028=VECTOR('',#4155,10.);
#1029=VECTOR('',#4156,10.);
#1030=VECTOR('',#4165,10.);
#1031=VECTOR('',#4168,10.);
#1032=VECTOR('',#4173,10.);
#1033=VECTOR('',#4176,10.);
#1034=VECTOR('',#4177,10.);
#1035=VECTOR('',#4178,10.);
#1036=VECTOR('',#4183,10.);
#1037=VECTOR('',#4184,10.);
#1038=VECTOR('',#4187,10.);
#1039=VECTOR('',#4188,10.);
#1040=VECTOR('',#4203,1.);
#1041=VECTOR('',#4206,10.);
#1042=VECTOR('',#4207,10.);
#1043=VECTOR('',#4208,10.);
#1044=VECTOR('',#4211,10.);
#1045=VECTOR('',#4214,10.);
#1046=VECTOR('',#4217,10.);
#1047=VECTOR('',#4218,10.);
#1048=VECTOR('',#4219,10.);
#1049=VECTOR('',#4222,10.);
#1050=VECTOR('',#4225,10.);
#1051=VECTOR('',#4226,10.);
#1052=VECTOR('',#4231,5.);
#1053=VECTOR('',#4238,10.);
#1054=VECTOR('',#4241,10.);
#1055=VECTOR('',#4246,10.);
#1056=VECTOR('',#4249,10.);
#1057=VECTOR('',#4254,10.);
#1058=VECTOR('',#4257,10.);
#1059=VECTOR('',#4272,10.);
#1060=VECTOR('',#4275,10.);
#1061=VECTOR('',#4278,10.);
#1062=VECTOR('',#4281,10.);
#1063=VECTOR('',#4284,10.);
#1064=VECTOR('',#4291,10.);
#1065=VECTOR('',#4292,10.);
#1066=VECTOR('',#4299,10.);
#1067=VECTOR('',#4300,10.);
#1068=VECTOR('',#4307,10.);
#1069=VECTOR('',#4312,7.);
#1070=VECTOR('',#4319,13.5);
#1071=VECTOR('',#4326,10.);
#1072=VECTOR('',#4329,10.);
#1073=VECTOR('',#4332,10.);
#1074=VECTOR('',#4337,10.);
#1075=VECTOR('',#4338,10.);
#1076=VECTOR('',#4339,10.);
#1077=VECTOR('',#4342,10.);
#1078=VECTOR('',#4343,10.);
#1079=VECTOR('',#4352,10.);
#1080=VECTOR('',#4355,10.);
#1081=VECTOR('',#4358,10.);
#1082=VECTOR('',#4363,10.);
#1083=VECTOR('',#4364,10.);
#1084=VECTOR('',#4365,10.);
#1085=VECTOR('',#4368,10.);
#1086=VECTOR('',#4369,10.);
#1087=VECTOR('',#4378,10.);
#1088=VECTOR('',#4381,10.);
#1089=VECTOR('',#4384,10.);
#1090=VECTOR('',#4389,10.);
#1091=VECTOR('',#4390,10.);
#1092=VECTOR('',#4391,10.);
#1093=VECTOR('',#4394,10.);
#1094=VECTOR('',#4397,10.);
#1095=VECTOR('',#4400,10.);
#1096=VECTOR('',#4401,10.);
#1097=VECTOR('',#4412,10.);
#1098=VECTOR('',#4413,10.);
#1099=VECTOR('',#4414,10.);
#1100=VECTOR('',#4415,10.);
#1101=VECTOR('',#4418,10.);
#1102=VECTOR('',#4419,10.);
#1103=VECTOR('',#4420,10.);
#1104=VECTOR('',#4423,10.);
#1105=VECTOR('',#4424,10.);
#1106=VECTOR('',#4425,10.);
#1107=VECTOR('',#4428,9.99999999999999);
#1108=VECTOR('',#4429,10.);
#1109=VECTOR('',#4430,9.99999999999999);
#1110=VECTOR('',#4433,10.);
#1111=VECTOR('',#4434,10.);
#1112=VECTOR('',#4435,10.);
#1113=VECTOR('',#4438,10.);
#1114=VECTOR('',#4439,10.);
#1115=VECTOR('',#4446,1.);
#1116=VECTOR('',#4457,10.);
#1117=VECTOR('',#4458,10.);
#1118=VECTOR('',#4459,10.);
#1119=VECTOR('',#4460,10.);
#1120=VECTOR('',#4463,10.);
#1121=VECTOR('',#4464,10.);
#1122=VECTOR('',#4465,10.);
#1123=VECTOR('',#4468,10.);
#1124=VECTOR('',#4469,10.);
#1125=VECTOR('',#4470,10.);
#1126=VECTOR('',#4473,9.99999999999999);
#1127=VECTOR('',#4474,9.99999999999999);
#1128=VECTOR('',#4475,10.);
#1129=VECTOR('',#4478,10.);
#1130=VECTOR('',#4479,10.);
#1131=VECTOR('',#4480,10.);
#1132=VECTOR('',#4483,10.);
#1133=VECTOR('',#4484,10.);
#1134=VECTOR('',#4491,1.);
#1135=VECTOR('',#4502,10.);
#1136=VECTOR('',#4503,10.);
#1137=VECTOR('',#4504,10.);
#1138=VECTOR('',#4505,10.);
#1139=VECTOR('',#4510,10.);
#1140=VECTOR('',#4515,10.);
#1141=VECTOR('',#4518,10.);
#1142=VECTOR('',#4519,10.);
#1143=VECTOR('',#4530,5.);
#1144=VECTOR('',#4537,10.);
#1145=VECTOR('',#4538,10.);
#1146=VECTOR('',#4539,10.);
#1147=VECTOR('',#4540,10.);
#1148=VECTOR('',#4543,10.);
#1149=VECTOR('',#4548,10.);
#1150=VECTOR('',#4553,10.);
#1151=VECTOR('',#4554,10.);
#1152=VECTOR('',#4563,5.);
#1153=VECTOR('',#4574,10.);
#1154=VECTOR('',#4577,10.);
#1155=VECTOR('',#4580,10.);
#1156=VECTOR('',#4581,10.);
#1157=VECTOR('',#4582,10.);
#1158=VECTOR('',#4587,10.);
#1159=VECTOR('',#4590,10.);
#1160=VECTOR('',#4595,10.);
#1161=VECTOR('',#4604,10.);
#1162=VECTOR('',#4607,10.);
#1163=VECTOR('',#4610,10.);
#1164=VECTOR('',#4611,10.);
#1165=VECTOR('',#4612,10.);
#1166=VECTOR('',#4615,10.);
#1167=VECTOR('',#4622,10.);
#1168=VECTOR('',#4625,10.);
#1169=CIRCLE('',#3400,1.);
#1170=CIRCLE('',#3401,1.);
#1171=CIRCLE('',#3404,1.);
#1172=CIRCLE('',#3405,1.);
#1173=CIRCLE('',#3408,1.);
#1174=CIRCLE('',#3409,1.);
#1175=CIRCLE('',#3412,1.);
#1176=CIRCLE('',#3413,1.);
#1177=CIRCLE('',#3416,1.);
#1178=CIRCLE('',#3417,1.);
#1179=CIRCLE('',#3420,1.);
#1180=CIRCLE('',#3421,1.);
#1181=CIRCLE('',#3424,1.);
#1182=CIRCLE('',#3425,1.);
#1183=CIRCLE('',#3428,1.);
#1184=CIRCLE('',#3429,1.);
#1185=CIRCLE('',#3432,1.);
#1186=CIRCLE('',#3433,1.);
#1187=CIRCLE('',#3436,1.);
#1188=CIRCLE('',#3437,1.);
#1189=CIRCLE('',#3440,11.9999999999996);
#1190=CIRCLE('',#3441,11.9999999999996);
#1191=CIRCLE('',#3443,11.9999999999996);
#1192=CIRCLE('',#3444,11.9999999999996);
#1193=CIRCLE('',#3446,11.9999999999996);
#1194=CIRCLE('',#3447,11.9999999999996);
#1195=CIRCLE('',#3449,11.9999999999996);
#1196=CIRCLE('',#3450,11.9999999999996);
#1197=CIRCLE('',#3452,11.9999999999996);
#1198=CIRCLE('',#3453,11.9999999999996);
#1199=CIRCLE('',#3455,5.529);
#1200=CIRCLE('',#3456,5.529);
#1201=CIRCLE('',#3457,5.529);
#1202=CIRCLE('',#3458,5.529);
#1203=CIRCLE('',#3459,1.);
#1204=CIRCLE('',#3460,11.9999999999996);
#1205=CIRCLE('',#3461,1.);
#1206=CIRCLE('',#3462,5.529);
#1207=CIRCLE('',#3463,5.529);
#1208=CIRCLE('',#3464,5.);
#1209=CIRCLE('',#3466,5.529);
#1210=CIRCLE('',#3468,5.529);
#1211=CIRCLE('',#3470,5.529);
#1212=CIRCLE('',#3472,5.529);
#1213=CIRCLE('',#3474,5.529);
#1214=CIRCLE('',#3476,1.);
#1215=CIRCLE('',#3479,1.);
#1216=CIRCLE('',#3482,11.9999999999996);
#1217=CIRCLE('',#3484,5.529);
#1218=CIRCLE('',#3485,5.);
#1219=CIRCLE('',#3490,1.);
#1220=CIRCLE('',#3491,1.);
#1221=CIRCLE('',#3493,1.);
#1222=CIRCLE('',#3499,5.);
#1223=CIRCLE('',#3500,5.);
#1224=CIRCLE('',#3501,5.);
#1225=CIRCLE('',#3503,12.);
#1226=CIRCLE('',#3504,12.);
#1227=CIRCLE('',#3506,12.);
#1228=CIRCLE('',#3507,12.);
#1229=CIRCLE('',#3509,12.);
#1230=CIRCLE('',#3510,12.);
#1231=CIRCLE('',#3512,13.5);
#1232=CIRCLE('',#3513,12.);
#1233=CIRCLE('',#3514,12.);
#1234=CIRCLE('',#3515,12.);
#1235=CIRCLE('',#3517,12.);
#1236=CIRCLE('',#3519,12.);
#1237=CIRCLE('',#3521,1.);
#1238=CIRCLE('',#3522,5.529);
#1239=CIRCLE('',#3523,1.);
#1240=CIRCLE('',#3524,1.);
#1241=CIRCLE('',#3525,5.529);
#1242=CIRCLE('',#3526,1.);
#1243=CIRCLE('',#3527,1.);
#1244=CIRCLE('',#3528,5.529);
#1245=CIRCLE('',#3529,1.);
#1246=CIRCLE('',#3531,7.);
#1247=CIRCLE('',#3532,7.);
#1248=CIRCLE('',#3535,13.5);
#1249=CIRCLE('',#3538,5.529);
#1250=CIRCLE('',#3540,1.);
#1251=CIRCLE('',#3544,1.);
#1252=CIRCLE('',#3547,5.529);
#1253=CIRCLE('',#3549,1.);
#1254=CIRCLE('',#3553,1.);
#1255=CIRCLE('',#3556,5.529);
#1256=CIRCLE('',#3558,1.);
#1257=CIRCLE('',#3561,12.);
#1258=CIRCLE('',#3564,1.);
#1259=CIRCLE('',#3568,1.);
#1260=CIRCLE('',#3569,1.);
#1261=CIRCLE('',#3572,1.);
#1262=CIRCLE('',#3577,5.);
#1263=CIRCLE('',#3578,5.);
#1264=CIRCLE('',#3579,5.);
#1265=CIRCLE('',#3581,12.);
#1266=CIRCLE('',#3582,12.);
#1267=CIRCLE('',#3584,12.);
#1268=CIRCLE('',#3585,12.);
#1269=CIRCLE('',#3587,12.);
#1270=CIRCLE('',#3588,12.);
#1271=CIRCLE('',#3590,13.5);
#1272=CIRCLE('',#3591,12.);
#1273=CIRCLE('',#3592,12.);
#1274=CIRCLE('',#3593,12.);
#1275=CIRCLE('',#3595,12.);
#1276=CIRCLE('',#3597,12.);
#1277=CIRCLE('',#3599,1.);
#1278=CIRCLE('',#3600,5.529);
#1279=CIRCLE('',#3601,1.);
#1280=CIRCLE('',#3602,1.);
#1281=CIRCLE('',#3603,5.529);
#1282=CIRCLE('',#3604,1.);
#1283=CIRCLE('',#3605,1.);
#1284=CIRCLE('',#3606,5.529);
#1285=CIRCLE('',#3607,1.);
#1286=CIRCLE('',#3609,7.);
#1287=CIRCLE('',#3610,7.);
#1288=CIRCLE('',#3613,13.5);
#1289=CIRCLE('',#3616,5.529);
#1290=CIRCLE('',#3618,1.);
#1291=CIRCLE('',#3622,1.);
#1292=CIRCLE('',#3625,5.529);
#1293=CIRCLE('',#3627,1.);
#1294=CIRCLE('',#3631,1.);
#1295=CIRCLE('',#3634,5.529);
#1296=CIRCLE('',#3636,1.);
#1297=CIRCLE('',#3639,12.);
#1298=CIRCLE('',#3642,1.);
#1299=CIRCLE('',#3653,1.);
#1300=CIRCLE('',#3654,1.);
#1301=CIRCLE('',#3666,1.);
#1302=CIRCLE('',#3667,1.);
#1303=CIRCLE('',#3673,1.);
#1304=CIRCLE('',#3675,1.);
#1305=CIRCLE('',#3679,5.);
#1306=CIRCLE('',#3681,5.);
#1307=CIRCLE('',#3686,1.);
#1308=CIRCLE('',#3688,1.);
#1309=CIRCLE('',#3692,5.);
#1310=CIRCLE('',#3694,5.);
#1311=CIRCLE('',#3698,1.);
#1312=CIRCLE('',#3699,1.);
#1313=CIRCLE('',#3702,1.);
#1314=CIRCLE('',#3704,1.);
#1315=CIRCLE('',#3709,1.);
#1316=CIRCLE('',#3710,1.);
#1317=CIRCLE('',#3713,1.);
#1318=CIRCLE('',#3715,1.);
#1319=VERTEX_POINT('',#4649);
#1320=VERTEX_POINT('',#4650);
#1321=VERTEX_POINT('',#4652);
#1322=VERTEX_POINT('',#4654);
#1323=VERTEX_POINT('',#4658);
#1324=VERTEX_POINT('',#4660);
#1325=VERTEX_POINT('',#4664);
#1326=VERTEX_POINT('',#4665);
#1327=VERTEX_POINT('',#4667);
#1328=VERTEX_POINT('',#4669);
#1329=VERTEX_POINT('',#4673);
#1330=VERTEX_POINT('',#4675);
#1331=VERTEX_POINT('',#4679);
#1332=VERTEX_POINT('',#4680);
#1333=VERTEX_POINT('',#4682);
#1334=VERTEX_POINT('',#4684);
#1335=VERTEX_POINT('',#4688);
#1336=VERTEX_POINT('',#4690);
#1337=VERTEX_POINT('',#4694);
#1338=VERTEX_POINT('',#4695);
#1339=VERTEX_POINT('',#4697);
#1340=VERTEX_POINT('',#4699);
#1341=VERTEX_POINT('',#4703);
#1342=VERTEX_POINT('',#4705);
#1343=VERTEX_POINT('',#4709);
#1344=VERTEX_POINT('',#4710);
#1345=VERTEX_POINT('',#4712);
#1346=VERTEX_POINT('',#4714);
#1347=VERTEX_POINT('',#4718);
#1348=VERTEX_POINT('',#4720);
#1349=VERTEX_POINT('',#4724);
#1350=VERTEX_POINT('',#4725);
#1351=VERTEX_POINT('',#4727);
#1352=VERTEX_POINT('',#4729);
#1353=VERTEX_POINT('',#4733);
#1354=VERTEX_POINT('',#4735);
#1355=VERTEX_POINT('',#4739);
#1356=VERTEX_POINT('',#4740);
#1357=VERTEX_POINT('',#4742);
#1358=VERTEX_POINT('',#4744);
#1359=VERTEX_POINT('',#4748);
#1360=VERTEX_POINT('',#4750);
#1361=VERTEX_POINT('',#4754);
#1362=VERTEX_POINT('',#4755);
#1363=VERTEX_POINT('',#4757);
#1364=VERTEX_POINT('',#4759);
#1365=VERTEX_POINT('',#4763);
#1366=VERTEX_POINT('',#4765);
#1367=VERTEX_POINT('',#4769);
#1368=VERTEX_POINT('',#4770);
#1369=VERTEX_POINT('',#4772);
#1370=VERTEX_POINT('',#4774);
#1371=VERTEX_POINT('',#4778);
#1372=VERTEX_POINT('',#4780);
#1373=VERTEX_POINT('',#4784);
#1374=VERTEX_POINT('',#4785);
#1375=VERTEX_POINT('',#4787);
#1376=VERTEX_POINT('',#4789);
#1377=VERTEX_POINT('',#4793);
#1378=VERTEX_POINT('',#4795);
#1379=VERTEX_POINT('',#4948);
#1380=VERTEX_POINT('',#5024);
#1381=VERTEX_POINT('',#5102);
#1382=VERTEX_POINT('',#5104);
#1383=VERTEX_POINT('',#5557);
#1384=VERTEX_POINT('',#5633);
#1385=VERTEX_POINT('',#5711);
#1386=VERTEX_POINT('',#5713);
#1387=VERTEX_POINT('',#6166);
#1388=VERTEX_POINT('',#6242);
#1389=VERTEX_POINT('',#6320);
#1390=VERTEX_POINT('',#6322);
#1391=VERTEX_POINT('',#6775);
#1392=VERTEX_POINT('',#6851);
#1393=VERTEX_POINT('',#6929);
#1394=VERTEX_POINT('',#6931);
#1395=VERTEX_POINT('',#7384);
#1396=VERTEX_POINT('',#7460);
#1397=VERTEX_POINT('',#7538);
#1398=VERTEX_POINT('',#7540);
#1399=VERTEX_POINT('',#7847);
#1400=VERTEX_POINT('',#7849);
#1401=VERTEX_POINT('',#7851);
#1402=VERTEX_POINT('',#7853);
#1403=VERTEX_POINT('',#7929);
#1404=VERTEX_POINT('',#7931);
#1405=VERTEX_POINT('',#8007);
#1406=VERTEX_POINT('',#8009);
#1407=VERTEX_POINT('',#8013);
#1408=VERTEX_POINT('',#8016);
#1409=VERTEX_POINT('',#8028);
#1410=VERTEX_POINT('',#8032);
#1411=VERTEX_POINT('',#8036);
#1412=VERTEX_POINT('',#8038);
#1413=VERTEX_POINT('',#8042);
#1414=VERTEX_POINT('',#8195);
#1415=VERTEX_POINT('',#8273);
#1416=VERTEX_POINT('',#8503);
#1417=VERTEX_POINT('',#8510);
#1418=VERTEX_POINT('',#8511);
#1419=VERTEX_POINT('',#8514);
#1420=VERTEX_POINT('',#8516);
#1421=VERTEX_POINT('',#8554);
#1422=VERTEX_POINT('',#8556);
#1423=VERTEX_POINT('',#8560);
#1424=VERTEX_POINT('',#8562);
#1425=VERTEX_POINT('',#8566);
#1426=VERTEX_POINT('',#8567);
#1427=VERTEX_POINT('',#8589);
#1428=VERTEX_POINT('',#8593);
#1429=VERTEX_POINT('',#8597);
#1430=VERTEX_POINT('',#8599);
#1431=VERTEX_POINT('',#8604);
#1432=VERTEX_POINT('',#8605);
#1433=VERTEX_POINT('',#8607);
#1434=VERTEX_POINT('',#8609);
#1435=VERTEX_POINT('',#8613);
#1436=VERTEX_POINT('',#8614);
#1437=VERTEX_POINT('',#8616);
#1438=VERTEX_POINT('',#8618);
#1439=VERTEX_POINT('',#8622);
#1440=VERTEX_POINT('',#8623);
#1441=VERTEX_POINT('',#8625);
#1442=VERTEX_POINT('',#8627);
#1443=VERTEX_POINT('',#8631);
#1444=VERTEX_POINT('',#8637);
#1445=VERTEX_POINT('',#8639);
#1446=VERTEX_POINT('',#8643);
#1447=VERTEX_POINT('',#8645);
#1448=VERTEX_POINT('',#8649);
#1449=VERTEX_POINT('',#8660);
#1450=VERTEX_POINT('',#8662);
#1451=VERTEX_POINT('',#8664);
#1452=VERTEX_POINT('',#8666);
#1453=VERTEX_POINT('',#8668);
#1454=VERTEX_POINT('',#8680);
#1455=VERTEX_POINT('',#8691);
#1456=VERTEX_POINT('',#8693);
#1457=VERTEX_POINT('',#8695);
#1458=VERTEX_POINT('',#8697);
#1459=VERTEX_POINT('',#8699);
#1460=VERTEX_POINT('',#8711);
#1461=VERTEX_POINT('',#8722);
#1462=VERTEX_POINT('',#8724);
#1463=VERTEX_POINT('',#8726);
#1464=VERTEX_POINT('',#8728);
#1465=VERTEX_POINT('',#8730);
#1466=VERTEX_POINT('',#8743);
#1467=VERTEX_POINT('',#8745);
#1468=VERTEX_POINT('',#8750);
#1469=VERTEX_POINT('',#8755);
#1470=VERTEX_POINT('',#8757);
#1471=VERTEX_POINT('',#8761);
#1472=VERTEX_POINT('',#8765);
#1473=VERTEX_POINT('',#8818);
#1474=VERTEX_POINT('',#8831);
#1475=VERTEX_POINT('',#8838);
#1476=VERTEX_POINT('',#8840);
#1477=VERTEX_POINT('',#8844);
#1478=VERTEX_POINT('',#8848);
#1479=VERTEX_POINT('',#8901);
#1480=VERTEX_POINT('',#8914);
#1481=VERTEX_POINT('',#8921);
#1482=VERTEX_POINT('',#8923);
#1483=VERTEX_POINT('',#8927);
#1484=VERTEX_POINT('',#8931);
#1485=VERTEX_POINT('',#8954);
#1486=VERTEX_POINT('',#8967);
#1487=VERTEX_POINT('',#8990);
#1488=VERTEX_POINT('',#9003);
#1489=VERTEX_POINT('',#9011);
#1490=VERTEX_POINT('',#9012);
#1491=VERTEX_POINT('',#9015);
#1492=VERTEX_POINT('',#9017);
#1493=VERTEX_POINT('',#9055);
#1494=VERTEX_POINT('',#9057);
#1495=VERTEX_POINT('',#9061);
#1496=VERTEX_POINT('',#9063);
#1497=VERTEX_POINT('',#9067);
#1498=VERTEX_POINT('',#9069);
#1499=VERTEX_POINT('',#9073);
#1500=VERTEX_POINT('',#9094);
#1501=VERTEX_POINT('',#9098);
#1502=VERTEX_POINT('',#9100);
#1503=VERTEX_POINT('',#9105);
#1504=VERTEX_POINT('',#9106);
#1505=VERTEX_POINT('',#9108);
#1506=VERTEX_POINT('',#9110);
#1507=VERTEX_POINT('',#9114);
#1508=VERTEX_POINT('',#9115);
#1509=VERTEX_POINT('',#9117);
#1510=VERTEX_POINT('',#9119);
#1511=VERTEX_POINT('',#9123);
#1512=VERTEX_POINT('',#9124);
#1513=VERTEX_POINT('',#9126);
#1514=VERTEX_POINT('',#9128);
#1515=VERTEX_POINT('',#9132);
#1516=VERTEX_POINT('',#9138);
#1517=VERTEX_POINT('',#9140);
#1518=VERTEX_POINT('',#9144);
#1519=VERTEX_POINT('',#9146);
#1520=VERTEX_POINT('',#9150);
#1521=VERTEX_POINT('',#9161);
#1522=VERTEX_POINT('',#9163);
#1523=VERTEX_POINT('',#9165);
#1524=VERTEX_POINT('',#9167);
#1525=VERTEX_POINT('',#9169);
#1526=VERTEX_POINT('',#9181);
#1527=VERTEX_POINT('',#9192);
#1528=VERTEX_POINT('',#9194);
#1529=VERTEX_POINT('',#9196);
#1530=VERTEX_POINT('',#9198);
#1531=VERTEX_POINT('',#9200);
#1532=VERTEX_POINT('',#9212);
#1533=VERTEX_POINT('',#9223);
#1534=VERTEX_POINT('',#9225);
#1535=VERTEX_POINT('',#9227);
#1536=VERTEX_POINT('',#9229);
#1537=VERTEX_POINT('',#9231);
#1538=VERTEX_POINT('',#9244);
#1539=VERTEX_POINT('',#9246);
#1540=VERTEX_POINT('',#9251);
#1541=VERTEX_POINT('',#9256);
#1542=VERTEX_POINT('',#9258);
#1543=VERTEX_POINT('',#9262);
#1544=VERTEX_POINT('',#9266);
#1545=VERTEX_POINT('',#9319);
#1546=VERTEX_POINT('',#9332);
#1547=VERTEX_POINT('',#9339);
#1548=VERTEX_POINT('',#9341);
#1549=VERTEX_POINT('',#9345);
#1550=VERTEX_POINT('',#9349);
#1551=VERTEX_POINT('',#9402);
#1552=VERTEX_POINT('',#9415);
#1553=VERTEX_POINT('',#9422);
#1554=VERTEX_POINT('',#9424);
#1555=VERTEX_POINT('',#9428);
#1556=VERTEX_POINT('',#9432);
#1557=VERTEX_POINT('',#9455);
#1558=VERTEX_POINT('',#9468);
#1559=VERTEX_POINT('',#9491);
#1560=VERTEX_POINT('',#9504);
#1561=VERTEX_POINT('',#9512);
#1562=VERTEX_POINT('',#9513);
#1563=VERTEX_POINT('',#9515);
#1564=VERTEX_POINT('',#9517);
#1565=VERTEX_POINT('',#9521);
#1566=VERTEX_POINT('',#9523);
#1567=VERTEX_POINT('',#9527);
#1568=VERTEX_POINT('',#9529);
#1569=VERTEX_POINT('',#9533);
#1570=VERTEX_POINT('',#9535);
#1571=VERTEX_POINT('',#9539);
#1572=VERTEX_POINT('',#9541);
#1573=VERTEX_POINT('',#9549);
#1574=VERTEX_POINT('',#9551);
#1575=VERTEX_POINT('',#9558);
#1576=VERTEX_POINT('',#9559);
#1577=VERTEX_POINT('',#9561);
#1578=VERTEX_POINT('',#9563);
#1579=VERTEX_POINT('',#9567);
#1580=VERTEX_POINT('',#9569);
#1581=VERTEX_POINT('',#9573);
#1582=VERTEX_POINT('',#9575);
#1583=VERTEX_POINT('',#9579);
#1584=VERTEX_POINT('',#9581);
#1585=VERTEX_POINT('',#9585);
#1586=VERTEX_POINT('',#9587);
#1587=VERTEX_POINT('',#9595);
#1588=VERTEX_POINT('',#9597);
#1589=VERTEX_POINT('',#9604);
#1590=VERTEX_POINT('',#9605);
#1591=VERTEX_POINT('',#9607);
#1592=VERTEX_POINT('',#9609);
#1593=VERTEX_POINT('',#9613);
#1594=VERTEX_POINT('',#9632);
#1595=VERTEX_POINT('',#9636);
#1596=VERTEX_POINT('',#9640);
#1597=VERTEX_POINT('',#9663);
#1598=VERTEX_POINT('',#9666);
#1599=VERTEX_POINT('',#9672);
#1600=VERTEX_POINT('',#9673);
#1601=VERTEX_POINT('',#9675);
#1602=VERTEX_POINT('',#9677);
#1603=VERTEX_POINT('',#9681);
#1604=VERTEX_POINT('',#9700);
#1605=VERTEX_POINT('',#9704);
#1606=VERTEX_POINT('',#9708);
#1607=VERTEX_POINT('',#9731);
#1608=VERTEX_POINT('',#9734);
#1609=VERTEX_POINT('',#9740);
#1610=VERTEX_POINT('',#9741);
#1611=VERTEX_POINT('',#9743);
#1612=VERTEX_POINT('',#9745);
#1613=VERTEX_POINT('',#9749);
#1614=VERTEX_POINT('',#9751);
#1615=VERTEX_POINT('',#9755);
#1616=VERTEX_POINT('',#9759);
#1617=VERTEX_POINT('',#9767);
#1618=VERTEX_POINT('',#9768);
#1619=VERTEX_POINT('',#9770);
#1620=VERTEX_POINT('',#9772);
#1621=VERTEX_POINT('',#9776);
#1622=VERTEX_POINT('',#9778);
#1623=VERTEX_POINT('',#9782);
#1624=VERTEX_POINT('',#9786);
#1625=EDGE_CURVE('',#1319,#1320,#1169,.F.);
#1626=EDGE_CURVE('',#1320,#1321,#651,.T.);
#1627=EDGE_CURVE('',#1321,#1322,#1170,.T.);
#1628=EDGE_CURVE('',#1322,#1319,#652,.T.);
#1629=EDGE_CURVE('',#1323,#1320,#653,.T.);
#1630=EDGE_CURVE('',#1324,#1323,#654,.T.);
#1631=EDGE_CURVE('',#1321,#1324,#655,.F.);
#1632=EDGE_CURVE('',#1325,#1326,#1171,.T.);
#1633=EDGE_CURVE('',#1326,#1327,#656,.T.);
#1634=EDGE_CURVE('',#1327,#1328,#1172,.F.);
#1635=EDGE_CURVE('',#1328,#1325,#657,.T.);
#1636=EDGE_CURVE('',#1326,#1329,#658,.T.);
#1637=EDGE_CURVE('',#1329,#1330,#659,.T.);
#1638=EDGE_CURVE('',#1327,#1330,#660,.T.);
#1639=EDGE_CURVE('',#1331,#1332,#1173,.F.);
#1640=EDGE_CURVE('',#1332,#1333,#661,.T.);
#1641=EDGE_CURVE('',#1333,#1334,#1174,.T.);
#1642=EDGE_CURVE('',#1334,#1331,#662,.T.);
#1643=EDGE_CURVE('',#1335,#1332,#663,.T.);
#1644=EDGE_CURVE('',#1336,#1335,#664,.T.);
#1645=EDGE_CURVE('',#1333,#1336,#665,.F.);
#1646=EDGE_CURVE('',#1337,#1338,#1175,.T.);
#1647=EDGE_CURVE('',#1338,#1339,#666,.T.);
#1648=EDGE_CURVE('',#1339,#1340,#1176,.F.);
#1649=EDGE_CURVE('',#1340,#1337,#667,.T.);
#1650=EDGE_CURVE('',#1338,#1341,#668,.T.);
#1651=EDGE_CURVE('',#1341,#1342,#669,.T.);
#1652=EDGE_CURVE('',#1339,#1342,#670,.T.);
#1653=EDGE_CURVE('',#1343,#1344,#1177,.F.);
#1654=EDGE_CURVE('',#1344,#1345,#671,.T.);
#1655=EDGE_CURVE('',#1345,#1346,#1178,.T.);
#1656=EDGE_CURVE('',#1346,#1343,#672,.T.);
#1657=EDGE_CURVE('',#1347,#1344,#673,.T.);
#1658=EDGE_CURVE('',#1348,#1347,#674,.T.);
#1659=EDGE_CURVE('',#1345,#1348,#675,.F.);
#1660=EDGE_CURVE('',#1349,#1350,#1179,.T.);
#1661=EDGE_CURVE('',#1350,#1351,#676,.T.);
#1662=EDGE_CURVE('',#1351,#1352,#1180,.F.);
#1663=EDGE_CURVE('',#1352,#1349,#677,.T.);
#1664=EDGE_CURVE('',#1350,#1353,#678,.T.);
#1665=EDGE_CURVE('',#1353,#1354,#679,.T.);
#1666=EDGE_CURVE('',#1351,#1354,#680,.T.);
#1667=EDGE_CURVE('',#1355,#1356,#1181,.F.);
#1668=EDGE_CURVE('',#1356,#1357,#681,.T.);
#1669=EDGE_CURVE('',#1357,#1358,#1182,.T.);
#1670=EDGE_CURVE('',#1358,#1355,#682,.T.);
#1671=EDGE_CURVE('',#1359,#1356,#683,.T.);
#1672=EDGE_CURVE('',#1360,#1359,#684,.T.);
#1673=EDGE_CURVE('',#1357,#1360,#685,.F.);
#1674=EDGE_CURVE('',#1361,#1362,#1183,.T.);
#1675=EDGE_CURVE('',#1362,#1363,#686,.T.);
#1676=EDGE_CURVE('',#1363,#1364,#1184,.F.);
#1677=EDGE_CURVE('',#1364,#1361,#687,.T.);
#1678=EDGE_CURVE('',#1362,#1365,#688,.T.);
#1679=EDGE_CURVE('',#1365,#1366,#689,.T.);
#1680=EDGE_CURVE('',#1363,#1366,#690,.T.);
#1681=EDGE_CURVE('',#1367,#1368,#1185,.F.);
#1682=EDGE_CURVE('',#1368,#1369,#691,.T.);
#1683=EDGE_CURVE('',#1369,#1370,#1186,.T.);
#1684=EDGE_CURVE('',#1370,#1367,#692,.T.);
#1685=EDGE_CURVE('',#1371,#1368,#693,.T.);
#1686=EDGE_CURVE('',#1372,#1371,#694,.T.);
#1687=EDGE_CURVE('',#1369,#1372,#695,.F.);
#1688=EDGE_CURVE('',#1373,#1374,#1187,.T.);
#1689=EDGE_CURVE('',#1374,#1375,#696,.T.);
#1690=EDGE_CURVE('',#1375,#1376,#1188,.F.);
#1691=EDGE_CURVE('',#1376,#1373,#697,.T.);
#1692=EDGE_CURVE('',#1374,#1377,#698,.T.);
#1693=EDGE_CURVE('',#1377,#1378,#699,.T.);
#1694=EDGE_CURVE('',#1375,#1378,#700,.T.);
#1695=EDGE_CURVE('',#1324,#1379,#99,.F.);
#1696=EDGE_CURVE('',#1380,#1323,#100,.T.);
#1697=EDGE_CURVE('',#1379,#1380,#701,.T.);
#1698=EDGE_CURVE('',#1381,#1379,#1189,.T.);
#1699=EDGE_CURVE('',#1382,#1380,#1190,.T.);
#1700=EDGE_CURVE('',#1381,#1382,#702,.T.);
#1701=EDGE_CURVE('',#1329,#1381,#101,.T.);
#1702=EDGE_CURVE('',#1330,#1382,#102,.T.);
#1703=EDGE_CURVE('',#1336,#1383,#103,.F.);
#1704=EDGE_CURVE('',#1384,#1335,#104,.T.);
#1705=EDGE_CURVE('',#1383,#1384,#703,.T.);
#1706=EDGE_CURVE('',#1385,#1383,#1191,.T.);
#1707=EDGE_CURVE('',#1386,#1384,#1192,.T.);
#1708=EDGE_CURVE('',#1385,#1386,#704,.T.);
#1709=EDGE_CURVE('',#1341,#1385,#105,.T.);
#1710=EDGE_CURVE('',#1342,#1386,#106,.T.);
#1711=EDGE_CURVE('',#1348,#1387,#107,.F.);
#1712=EDGE_CURVE('',#1388,#1347,#108,.T.);
#1713=EDGE_CURVE('',#1387,#1388,#705,.T.);
#1714=EDGE_CURVE('',#1389,#1387,#1193,.T.);
#1715=EDGE_CURVE('',#1390,#1388,#1194,.T.);
#1716=EDGE_CURVE('',#1389,#1390,#706,.T.);
#1717=EDGE_CURVE('',#1353,#1389,#109,.T.);
#1718=EDGE_CURVE('',#1354,#1390,#110,.T.);
#1719=EDGE_CURVE('',#1360,#1391,#111,.F.);
#1720=EDGE_CURVE('',#1392,#1359,#112,.T.);
#1721=EDGE_CURVE('',#1391,#1392,#707,.T.);
#1722=EDGE_CURVE('',#1393,#1391,#1195,.T.);
#1723=EDGE_CURVE('',#1394,#1392,#1196,.T.);
#1724=EDGE_CURVE('',#1393,#1394,#708,.T.);
#1725=EDGE_CURVE('',#1365,#1393,#113,.T.);
#1726=EDGE_CURVE('',#1366,#1394,#114,.T.);
#1727=EDGE_CURVE('',#1372,#1395,#115,.F.);
#1728=EDGE_CURVE('',#1396,#1371,#116,.T.);
#1729=EDGE_CURVE('',#1395,#1396,#709,.T.);
#1730=EDGE_CURVE('',#1397,#1395,#1197,.T.);
#1731=EDGE_CURVE('',#1398,#1396,#1198,.T.);
#1732=EDGE_CURVE('',#1397,#1398,#710,.T.);
#1733=EDGE_CURVE('',#1377,#1397,#117,.T.);
#1734=EDGE_CURVE('',#1378,#1398,#118,.T.);
#1735=EDGE_CURVE('',#1346,#1337,#1199,.T.);
#1736=EDGE_CURVE('',#1358,#1349,#1200,.T.);
#1737=EDGE_CURVE('',#1370,#1361,#1201,.T.);
#1738=EDGE_CURVE('',#1399,#1373,#1202,.T.);
#1739=EDGE_CURVE('',#1400,#1399,#1203,.T.);
#1740=EDGE_CURVE('',#1400,#1401,#711,.F.);
#1741=EDGE_CURVE('',#1401,#1402,#119,.F.);
#1742=EDGE_CURVE('',#1403,#1402,#1204,.T.);
#1743=EDGE_CURVE('',#1404,#1403,#120,.T.);
#1744=EDGE_CURVE('',#1405,#1404,#712,.T.);
#1745=EDGE_CURVE('',#1406,#1405,#1205,.T.);
#1746=EDGE_CURVE('',#1322,#1406,#1206,.T.);
#1747=EDGE_CURVE('',#1334,#1325,#1207,.T.);
#1748=EDGE_CURVE('',#1407,#1407,#1208,.T.);
#1749=EDGE_CURVE('',#1408,#1376,#1209,.T.);
#1750=EDGE_CURVE('',#1399,#1408,#713,.T.);
#1751=EDGE_CURVE('',#1367,#1364,#1210,.T.);
#1752=EDGE_CURVE('',#1355,#1352,#1211,.T.);
#1753=EDGE_CURVE('',#1343,#1340,#1212,.T.);
#1754=EDGE_CURVE('',#1331,#1328,#1213,.T.);
#1755=EDGE_CURVE('',#1408,#1409,#1214,.F.);
#1756=EDGE_CURVE('',#1409,#1400,#714,.T.);
#1757=EDGE_CURVE('',#1410,#1409,#715,.T.);
#1758=EDGE_CURVE('',#1401,#1410,#716,.T.);
#1759=EDGE_CURVE('',#1405,#1411,#717,.T.);
#1760=EDGE_CURVE('',#1411,#1412,#1215,.F.);
#1761=EDGE_CURVE('',#1412,#1406,#718,.T.);
#1762=EDGE_CURVE('',#1404,#1413,#719,.T.);
#1763=EDGE_CURVE('',#1411,#1413,#720,.T.);
#1764=EDGE_CURVE('',#1414,#1410,#121,.T.);
#1765=EDGE_CURVE('',#1402,#1414,#721,.T.);
#1766=EDGE_CURVE('',#1415,#1414,#1216,.T.);
#1767=EDGE_CURVE('',#1403,#1415,#722,.T.);
#1768=EDGE_CURVE('',#1413,#1415,#122,.T.);
#1769=EDGE_CURVE('',#1319,#1412,#1217,.T.);
#1770=EDGE_CURVE('',#1416,#1416,#1218,.T.);
#1771=EDGE_CURVE('',#1407,#1416,#723,.T.);
#1772=EDGE_CURVE('',#1417,#1418,#1219,.T.);
#1773=EDGE_CURVE('',#1418,#1417,#1220,.T.);
#1774=EDGE_CURVE('',#1418,#1419,#724,.T.);
#1775=EDGE_CURVE('',#1420,#1419,#123,.T.);
#1776=EDGE_CURVE('',#1419,#1420,#124,.T.);
#1777=EDGE_CURVE('',#1421,#1417,#725,.T.);
#1778=EDGE_CURVE('',#1422,#1421,#1221,.T.);
#1779=EDGE_CURVE('',#1418,#1422,#726,.T.);
#1780=EDGE_CURVE('',#1423,#1418,#727,.T.);
#1781=EDGE_CURVE('',#1424,#1423,#728,.T.);
#1782=EDGE_CURVE('',#1417,#1424,#729,.T.);
#1783=EDGE_CURVE('',#1425,#1426,#125,.T.);
#1784=EDGE_CURVE('',#1425,#1422,#730,.T.);
#1785=EDGE_CURVE('',#1426,#1421,#731,.T.);
#1786=EDGE_CURVE('',#1426,#1427,#732,.T.);
#1787=EDGE_CURVE('',#1427,#1424,#733,.T.);
#1788=EDGE_CURVE('',#1428,#1425,#734,.T.);
#1789=EDGE_CURVE('',#1423,#1428,#735,.T.);
#1790=EDGE_CURVE('',#1429,#1429,#1222,.T.);
#1791=EDGE_CURVE('',#1429,#1430,#736,.T.);
#1792=EDGE_CURVE('',#1428,#1430,#1223,.T.);
#1793=EDGE_CURVE('',#1430,#1427,#1224,.T.);
#1794=EDGE_CURVE('',#1431,#1432,#737,.T.);
#1795=EDGE_CURVE('',#1433,#1431,#1225,.T.);
#1796=EDGE_CURVE('',#1433,#1434,#738,.T.);
#1797=EDGE_CURVE('',#1432,#1434,#1226,.T.);
#1798=EDGE_CURVE('',#1435,#1436,#739,.T.);
#1799=EDGE_CURVE('',#1437,#1436,#1227,.T.);
#1800=EDGE_CURVE('',#1438,#1437,#740,.T.);
#1801=EDGE_CURVE('',#1435,#1438,#1228,.T.);
#1802=EDGE_CURVE('',#1439,#1440,#741,.T.);
#1803=EDGE_CURVE('',#1441,#1440,#1229,.T.);
#1804=EDGE_CURVE('',#1442,#1441,#742,.T.);
#1805=EDGE_CURVE('',#1439,#1442,#1230,.T.);
#1806=EDGE_CURVE('',#1443,#1443,#1231,.T.);
#1807=EDGE_CURVE('',#1441,#1436,#1232,.T.);
#1808=EDGE_CURVE('',#1432,#1440,#1233,.T.);
#1809=EDGE_CURVE('',#1437,#1434,#1234,.T.);
#1810=EDGE_CURVE('',#1436,#1444,#743,.T.);
#1811=EDGE_CURVE('',#1445,#1444,#1235,.T.);
#1812=EDGE_CURVE('',#1441,#1445,#744,.T.);
#1813=EDGE_CURVE('',#1434,#1446,#745,.T.);
#1814=EDGE_CURVE('',#1447,#1446,#1236,.T.);
#1815=EDGE_CURVE('',#1437,#1447,#746,.T.);
#1816=EDGE_CURVE('',#1448,#1442,#126,.T.);
#1817=EDGE_CURVE('',#1449,#1448,#747,.T.);
#1818=EDGE_CURVE('',#1449,#1450,#1237,.T.);
#1819=EDGE_CURVE('',#1451,#1450,#1238,.T.);
#1820=EDGE_CURVE('',#1451,#1452,#1239,.T.);
#1821=EDGE_CURVE('',#1453,#1452,#748,.T.);
#1822=EDGE_CURVE('',#1435,#1453,#127,.T.);
#1823=EDGE_CURVE('',#1454,#1438,#128,.T.);
#1824=EDGE_CURVE('',#1455,#1454,#749,.T.);
#1825=EDGE_CURVE('',#1455,#1456,#1240,.T.);
#1826=EDGE_CURVE('',#1457,#1456,#1241,.T.);
#1827=EDGE_CURVE('',#1457,#1458,#1242,.T.);
#1828=EDGE_CURVE('',#1459,#1458,#750,.T.);
#1829=EDGE_CURVE('',#1433,#1459,#129,.T.);
#1830=EDGE_CURVE('',#1460,#1431,#130,.T.);
#1831=EDGE_CURVE('',#1461,#1460,#751,.T.);
#1832=EDGE_CURVE('',#1461,#1462,#1243,.T.);
#1833=EDGE_CURVE('',#1463,#1462,#1244,.T.);
#1834=EDGE_CURVE('',#1463,#1464,#1245,.T.);
#1835=EDGE_CURVE('',#1465,#1464,#752,.T.);
#1836=EDGE_CURVE('',#1439,#1465,#131,.T.);
#1837=EDGE_CURVE('',#1466,#1466,#1246,.F.);
#1838=EDGE_CURVE('',#1466,#1467,#753,.T.);
#1839=EDGE_CURVE('',#1467,#1467,#1247,.T.);
#1840=EDGE_CURVE('',#1468,#1468,#1248,.T.);
#1841=EDGE_CURVE('',#1468,#1443,#754,.T.);
#1842=EDGE_CURVE('',#1450,#1469,#755,.T.);
#1843=EDGE_CURVE('',#1470,#1469,#1249,.T.);
#1844=EDGE_CURVE('',#1451,#1470,#756,.T.);
#1845=EDGE_CURVE('',#1471,#1470,#1250,.T.);
#1846=EDGE_CURVE('',#1452,#1471,#757,.T.);
#1847=EDGE_CURVE('',#1472,#1471,#758,.T.);
#1848=EDGE_CURVE('',#1453,#1472,#759,.T.);
#1849=EDGE_CURVE('',#1444,#1472,#132,.T.);
#1850=EDGE_CURVE('',#1473,#1445,#133,.T.);
#1851=EDGE_CURVE('',#1448,#1473,#760,.T.);
#1852=EDGE_CURVE('',#1474,#1473,#761,.T.);
#1853=EDGE_CURVE('',#1449,#1474,#762,.T.);
#1854=EDGE_CURVE('',#1469,#1474,#1251,.T.);
#1855=EDGE_CURVE('',#1456,#1475,#763,.T.);
#1856=EDGE_CURVE('',#1476,#1475,#1252,.T.);
#1857=EDGE_CURVE('',#1457,#1476,#764,.T.);
#1858=EDGE_CURVE('',#1477,#1476,#1253,.T.);
#1859=EDGE_CURVE('',#1458,#1477,#765,.T.);
#1860=EDGE_CURVE('',#1478,#1477,#766,.T.);
#1861=EDGE_CURVE('',#1459,#1478,#767,.T.);
#1862=EDGE_CURVE('',#1446,#1478,#134,.T.);
#1863=EDGE_CURVE('',#1479,#1447,#135,.T.);
#1864=EDGE_CURVE('',#1454,#1479,#768,.T.);
#1865=EDGE_CURVE('',#1480,#1479,#769,.T.);
#1866=EDGE_CURVE('',#1455,#1480,#770,.T.);
#1867=EDGE_CURVE('',#1475,#1480,#1254,.T.);
#1868=EDGE_CURVE('',#1462,#1481,#771,.T.);
#1869=EDGE_CURVE('',#1482,#1481,#1255,.T.);
#1870=EDGE_CURVE('',#1463,#1482,#772,.T.);
#1871=EDGE_CURVE('',#1483,#1482,#1256,.T.);
#1872=EDGE_CURVE('',#1464,#1483,#773,.T.);
#1873=EDGE_CURVE('',#1484,#1483,#774,.T.);
#1874=EDGE_CURVE('',#1465,#1484,#775,.T.);
#1875=EDGE_CURVE('',#1485,#1484,#136,.T.);
#1876=EDGE_CURVE('',#1440,#1485,#776,.T.);
#1877=EDGE_CURVE('',#1486,#1485,#1257,.T.);
#1878=EDGE_CURVE('',#1432,#1486,#777,.T.);
#1879=EDGE_CURVE('',#1487,#1486,#137,.T.);
#1880=EDGE_CURVE('',#1460,#1487,#778,.T.);
#1881=EDGE_CURVE('',#1488,#1487,#779,.T.);
#1882=EDGE_CURVE('',#1461,#1488,#780,.T.);
#1883=EDGE_CURVE('',#1481,#1488,#1258,.T.);
#1884=EDGE_CURVE('',#1489,#1490,#1259,.T.);
#1885=EDGE_CURVE('',#1490,#1489,#1260,.T.);
#1886=EDGE_CURVE('',#1490,#1491,#781,.T.);
#1887=EDGE_CURVE('',#1492,#1491,#138,.T.);
#1888=EDGE_CURVE('',#1491,#1492,#139,.T.);
#1889=EDGE_CURVE('',#1489,#1493,#782,.T.);
#1890=EDGE_CURVE('',#1494,#1493,#783,.T.);
#1891=EDGE_CURVE('',#1494,#1490,#784,.T.);
#1892=EDGE_CURVE('',#1490,#1495,#785,.T.);
#1893=EDGE_CURVE('',#1495,#1496,#1261,.T.);
#1894=EDGE_CURVE('',#1496,#1489,#786,.T.);
#1895=EDGE_CURVE('',#1493,#1497,#787,.T.);
#1896=EDGE_CURVE('',#1498,#1496,#788,.T.);
#1897=EDGE_CURVE('',#1497,#1498,#789,.T.);
#1898=EDGE_CURVE('',#1498,#1499,#140,.T.);
#1899=EDGE_CURVE('',#1499,#1495,#790,.T.);
#1900=EDGE_CURVE('',#1500,#1494,#791,.T.);
#1901=EDGE_CURVE('',#1499,#1500,#792,.T.);
#1902=EDGE_CURVE('',#1500,#1501,#1262,.T.);
#1903=EDGE_CURVE('',#1501,#1502,#793,.T.);
#1904=EDGE_CURVE('',#1502,#1502,#1263,.T.);
#1905=EDGE_CURVE('',#1501,#1497,#1264,.T.);
#1906=EDGE_CURVE('',#1503,#1504,#794,.T.);
#1907=EDGE_CURVE('',#1504,#1505,#1265,.T.);
#1908=EDGE_CURVE('',#1506,#1505,#795,.T.);
#1909=EDGE_CURVE('',#1506,#1503,#1266,.T.);
#1910=EDGE_CURVE('',#1507,#1508,#796,.T.);
#1911=EDGE_CURVE('',#1507,#1509,#1267,.T.);
#1912=EDGE_CURVE('',#1509,#1510,#797,.T.);
#1913=EDGE_CURVE('',#1510,#1508,#1268,.T.);
#1914=EDGE_CURVE('',#1511,#1512,#798,.T.);
#1915=EDGE_CURVE('',#1511,#1513,#1269,.T.);
#1916=EDGE_CURVE('',#1513,#1514,#799,.T.);
#1917=EDGE_CURVE('',#1514,#1512,#1270,.T.);
#1918=EDGE_CURVE('',#1515,#1515,#1271,.T.);
#1919=EDGE_CURVE('',#1514,#1508,#1272,.T.);
#1920=EDGE_CURVE('',#1510,#1505,#1273,.T.);
#1921=EDGE_CURVE('',#1504,#1512,#1274,.T.);
#1922=EDGE_CURVE('',#1514,#1516,#800,.T.);
#1923=EDGE_CURVE('',#1516,#1517,#1275,.T.);
#1924=EDGE_CURVE('',#1508,#1517,#801,.T.);
#1925=EDGE_CURVE('',#1510,#1518,#802,.T.);
#1926=EDGE_CURVE('',#1518,#1519,#1276,.T.);
#1927=EDGE_CURVE('',#1505,#1519,#803,.T.);
#1928=EDGE_CURVE('',#1511,#1520,#141,.T.);
#1929=EDGE_CURVE('',#1520,#1521,#804,.T.);
#1930=EDGE_CURVE('',#1522,#1521,#1277,.T.);
#1931=EDGE_CURVE('',#1522,#1523,#1278,.T.);
#1932=EDGE_CURVE('',#1524,#1523,#1279,.T.);
#1933=EDGE_CURVE('',#1524,#1525,#805,.T.);
#1934=EDGE_CURVE('',#1525,#1503,#142,.T.);
#1935=EDGE_CURVE('',#1506,#1526,#143,.T.);
#1936=EDGE_CURVE('',#1526,#1527,#806,.T.);
#1937=EDGE_CURVE('',#1528,#1527,#1280,.T.);
#1938=EDGE_CURVE('',#1528,#1529,#1281,.T.);
#1939=EDGE_CURVE('',#1530,#1529,#1282,.T.);
#1940=EDGE_CURVE('',#1530,#1531,#807,.T.);
#1941=EDGE_CURVE('',#1531,#1509,#144,.T.);
#1942=EDGE_CURVE('',#1507,#1532,#145,.T.);
#1943=EDGE_CURVE('',#1532,#1533,#808,.T.);
#1944=EDGE_CURVE('',#1534,#1533,#1283,.T.);
#1945=EDGE_CURVE('',#1534,#1535,#1284,.T.);
#1946=EDGE_CURVE('',#1536,#1535,#1285,.T.);
#1947=EDGE_CURVE('',#1536,#1537,#809,.T.);
#1948=EDGE_CURVE('',#1537,#1513,#146,.T.);
#1949=EDGE_CURVE('',#1538,#1538,#1286,.F.);
#1950=EDGE_CURVE('',#1538,#1539,#810,.T.);
#1951=EDGE_CURVE('',#1539,#1539,#1287,.T.);
#1952=EDGE_CURVE('',#1515,#1540,#811,.T.);
#1953=EDGE_CURVE('',#1540,#1540,#1288,.T.);
#1954=EDGE_CURVE('',#1534,#1541,#812,.T.);
#1955=EDGE_CURVE('',#1541,#1542,#1289,.T.);
#1956=EDGE_CURVE('',#1535,#1542,#813,.T.);
#1957=EDGE_CURVE('',#1533,#1543,#814,.T.);
#1958=EDGE_CURVE('',#1543,#1541,#1290,.T.);
#1959=EDGE_CURVE('',#1532,#1544,#815,.T.);
#1960=EDGE_CURVE('',#1544,#1543,#816,.T.);
#1961=EDGE_CURVE('',#1517,#1544,#147,.T.);
#1962=EDGE_CURVE('',#1537,#1545,#817,.T.);
#1963=EDGE_CURVE('',#1545,#1516,#148,.T.);
#1964=EDGE_CURVE('',#1536,#1546,#818,.T.);
#1965=EDGE_CURVE('',#1546,#1545,#819,.T.);
#1966=EDGE_CURVE('',#1542,#1546,#1291,.T.);
#1967=EDGE_CURVE('',#1528,#1547,#820,.T.);
#1968=EDGE_CURVE('',#1547,#1548,#1292,.T.);
#1969=EDGE_CURVE('',#1529,#1548,#821,.T.);
#1970=EDGE_CURVE('',#1527,#1549,#822,.T.);
#1971=EDGE_CURVE('',#1549,#1547,#1293,.T.);
#1972=EDGE_CURVE('',#1526,#1550,#823,.T.);
#1973=EDGE_CURVE('',#1550,#1549,#824,.T.);
#1974=EDGE_CURVE('',#1519,#1550,#149,.T.);
#1975=EDGE_CURVE('',#1531,#1551,#825,.T.);
#1976=EDGE_CURVE('',#1551,#1518,#150,.T.);
#1977=EDGE_CURVE('',#1530,#1552,#826,.T.);
#1978=EDGE_CURVE('',#1552,#1551,#827,.T.);
#1979=EDGE_CURVE('',#1548,#1552,#1294,.T.);
#1980=EDGE_CURVE('',#1522,#1553,#828,.T.);
#1981=EDGE_CURVE('',#1553,#1554,#1295,.T.);
#1982=EDGE_CURVE('',#1523,#1554,#829,.T.);
#1983=EDGE_CURVE('',#1521,#1555,#830,.T.);
#1984=EDGE_CURVE('',#1555,#1553,#1296,.T.);
#1985=EDGE_CURVE('',#1520,#1556,#831,.T.);
#1986=EDGE_CURVE('',#1556,#1555,#832,.T.);
#1987=EDGE_CURVE('',#1512,#1557,#833,.T.);
#1988=EDGE_CURVE('',#1557,#1556,#151,.T.);
#1989=EDGE_CURVE('',#1504,#1558,#834,.T.);
#1990=EDGE_CURVE('',#1558,#1557,#1297,.T.);
#1991=EDGE_CURVE('',#1525,#1559,#835,.T.);
#1992=EDGE_CURVE('',#1559,#1558,#152,.T.);
#1993=EDGE_CURVE('',#1524,#1560,#836,.T.);
#1994=EDGE_CURVE('',#1560,#1559,#837,.T.);
#1995=EDGE_CURVE('',#1554,#1560,#1298,.T.);
#1996=EDGE_CURVE('',#1561,#1562,#838,.T.);
#1997=EDGE_CURVE('',#1561,#1563,#839,.T.);
#1998=EDGE_CURVE('',#1563,#1564,#840,.T.);
#1999=EDGE_CURVE('',#1562,#1564,#841,.T.);
#2000=EDGE_CURVE('',#1565,#1561,#842,.T.);
#2001=EDGE_CURVE('',#1565,#1566,#843,.T.);
#2002=EDGE_CURVE('',#1566,#1563,#844,.T.);
#2003=EDGE_CURVE('',#1567,#1565,#845,.T.);
#2004=EDGE_CURVE('',#1567,#1568,#846,.T.);
#2005=EDGE_CURVE('',#1568,#1566,#847,.T.);
#2006=EDGE_CURVE('',#1569,#1567,#848,.T.);
#2007=EDGE_CURVE('',#1569,#1570,#849,.T.);
#2008=EDGE_CURVE('',#1570,#1568,#850,.T.);
#2009=EDGE_CURVE('',#1571,#1569,#851,.T.);
#2010=EDGE_CURVE('',#1571,#1572,#852,.T.);
#2011=EDGE_CURVE('',#1572,#1570,#853,.T.);
#2012=EDGE_CURVE('',#1562,#1571,#854,.T.);
#2013=EDGE_CURVE('',#1564,#1572,#855,.T.);
#2014=EDGE_CURVE('',#1573,#1573,#1299,.T.);
#2015=EDGE_CURVE('',#1573,#1574,#856,.T.);
#2016=EDGE_CURVE('',#1574,#1574,#1300,.T.);
#2017=EDGE_CURVE('',#1575,#1576,#857,.T.);
#2018=EDGE_CURVE('',#1576,#1577,#858,.T.);
#2019=EDGE_CURVE('',#1578,#1577,#859,.T.);
#2020=EDGE_CURVE('',#1575,#1578,#860,.T.);
#2021=EDGE_CURVE('',#1579,#1575,#861,.T.);
#2022=EDGE_CURVE('',#1580,#1578,#862,.T.);
#2023=EDGE_CURVE('',#1579,#1580,#863,.T.);
#2024=EDGE_CURVE('',#1581,#1579,#864,.T.);
#2025=EDGE_CURVE('',#1582,#1580,#865,.T.);
#2026=EDGE_CURVE('',#1581,#1582,#866,.T.);
#2027=EDGE_CURVE('',#1583,#1581,#867,.T.);
#2028=EDGE_CURVE('',#1584,#1582,#868,.T.);
#2029=EDGE_CURVE('',#1583,#1584,#869,.T.);
#2030=EDGE_CURVE('',#1585,#1583,#870,.T.);
#2031=EDGE_CURVE('',#1586,#1584,#871,.T.);
#2032=EDGE_CURVE('',#1585,#1586,#872,.T.);
#2033=EDGE_CURVE('',#1576,#1585,#873,.T.);
#2034=EDGE_CURVE('',#1577,#1586,#874,.T.);
#2035=EDGE_CURVE('',#1587,#1587,#1301,.T.);
#2036=EDGE_CURVE('',#1587,#1588,#875,.T.);
#2037=EDGE_CURVE('',#1588,#1588,#1302,.T.);
#2038=EDGE_CURVE('',#1589,#1590,#876,.T.);
#2039=EDGE_CURVE('',#1591,#1589,#877,.T.);
#2040=EDGE_CURVE('',#1592,#1591,#878,.T.);
#2041=EDGE_CURVE('',#1592,#1590,#879,.T.);
#2042=EDGE_CURVE('',#1590,#1593,#153,.T.);
#2043=EDGE_CURVE('',#1594,#1592,#1303,.T.);
#2044=EDGE_CURVE('',#1594,#1593,#880,.T.);
#2045=EDGE_CURVE('',#1591,#1595,#1304,.T.);
#2046=EDGE_CURVE('',#1595,#1594,#881,.T.);
#2047=EDGE_CURVE('',#1593,#1596,#882,.T.);
#2048=EDGE_CURVE('',#1595,#1596,#883,.T.);
#2049=EDGE_CURVE('',#1596,#1589,#154,.T.);
#2050=EDGE_CURVE('',#1597,#1597,#1305,.T.);
#2051=EDGE_CURVE('',#1598,#1598,#1306,.T.);
#2052=EDGE_CURVE('',#1598,#1597,#884,.T.);
#2053=EDGE_CURVE('',#1599,#1600,#885,.T.);
#2054=EDGE_CURVE('',#1601,#1600,#886,.T.);
#2055=EDGE_CURVE('',#1601,#1602,#887,.T.);
#2056=EDGE_CURVE('',#1602,#1599,#888,.T.);
#2057=EDGE_CURVE('',#1600,#1603,#155,.T.);
#2058=EDGE_CURVE('',#1604,#1603,#889,.T.);
#2059=EDGE_CURVE('',#1604,#1601,#1307,.T.);
#2060=EDGE_CURVE('',#1605,#1604,#890,.T.);
#2061=EDGE_CURVE('',#1602,#1605,#1308,.T.);
#2062=EDGE_CURVE('',#1603,#1606,#891,.T.);
#2063=EDGE_CURVE('',#1605,#1606,#892,.T.);
#2064=EDGE_CURVE('',#1606,#1599,#156,.T.);
#2065=EDGE_CURVE('',#1607,#1607,#1309,.T.);
#2066=EDGE_CURVE('',#1607,#1608,#893,.T.);
#2067=EDGE_CURVE('',#1608,#1608,#1310,.T.);
#2068=EDGE_CURVE('',#1609,#1610,#1311,.T.);
#2069=EDGE_CURVE('',#1610,#1611,#894,.T.);
#2070=EDGE_CURVE('',#1611,#1612,#1312,.T.);
#2071=EDGE_CURVE('',#1612,#1609,#895,.T.);
#2072=EDGE_CURVE('',#1612,#1613,#896,.T.);
#2073=EDGE_CURVE('',#1613,#1614,#897,.T.);
#2074=EDGE_CURVE('',#1609,#1614,#898,.T.);
#2075=EDGE_CURVE('',#1614,#1615,#1313,.T.);
#2076=EDGE_CURVE('',#1610,#1615,#899,.T.);
#2077=EDGE_CURVE('',#1611,#1616,#900,.T.);
#2078=EDGE_CURVE('',#1616,#1613,#1314,.T.);
#2079=EDGE_CURVE('',#1615,#1616,#901,.T.);
#2080=EDGE_CURVE('',#1617,#1618,#1315,.T.);
#2081=EDGE_CURVE('',#1619,#1617,#902,.T.);
#2082=EDGE_CURVE('',#1620,#1619,#1316,.T.);
#2083=EDGE_CURVE('',#1618,#1620,#903,.T.);
#2084=EDGE_CURVE('',#1617,#1621,#904,.T.);
#2085=EDGE_CURVE('',#1622,#1621,#905,.T.);
#2086=EDGE_CURVE('',#1619,#1622,#906,.T.);
#2087=EDGE_CURVE('',#1618,#1623,#907,.T.);
#2088=EDGE_CURVE('',#1621,#1623,#1317,.T.);
#2089=EDGE_CURVE('',#1624,#1622,#1318,.T.);
#2090=EDGE_CURVE('',#1620,#1624,#908,.T.);
#2091=EDGE_CURVE('',#1623,#1624,#909,.T.);
#2092=ORIENTED_EDGE('',*,*,#1625,.T.);
#2093=ORIENTED_EDGE('',*,*,#1626,.T.);
#2094=ORIENTED_EDGE('',*,*,#1627,.T.);
#2095=ORIENTED_EDGE('',*,*,#1628,.T.);
#2096=ORIENTED_EDGE('',*,*,#1626,.F.);
#2097=ORIENTED_EDGE('',*,*,#1629,.F.);
#2098=ORIENTED_EDGE('',*,*,#1630,.F.);
#2099=ORIENTED_EDGE('',*,*,#1631,.F.);
#2100=ORIENTED_EDGE('',*,*,#1632,.T.);
#2101=ORIENTED_EDGE('',*,*,#1633,.T.);
#2102=ORIENTED_EDGE('',*,*,#1634,.T.);
#2103=ORIENTED_EDGE('',*,*,#1635,.T.);
#2104=ORIENTED_EDGE('',*,*,#1633,.F.);
#2105=ORIENTED_EDGE('',*,*,#1636,.T.);
#2106=ORIENTED_EDGE('',*,*,#1637,.T.);
#2107=ORIENTED_EDGE('',*,*,#1638,.F.);
#2108=ORIENTED_EDGE('',*,*,#1639,.T.);
#2109=ORIENTED_EDGE('',*,*,#1640,.T.);
#2110=ORIENTED_EDGE('',*,*,#1641,.T.);
#2111=ORIENTED_EDGE('',*,*,#1642,.T.);
#2112=ORIENTED_EDGE('',*,*,#1640,.F.);
#2113=ORIENTED_EDGE('',*,*,#1643,.F.);
#2114=ORIENTED_EDGE('',*,*,#1644,.F.);
#2115=ORIENTED_EDGE('',*,*,#1645,.F.);
#2116=ORIENTED_EDGE('',*,*,#1646,.T.);
#2117=ORIENTED_EDGE('',*,*,#1647,.T.);
#2118=ORIENTED_EDGE('',*,*,#1648,.T.);
#2119=ORIENTED_EDGE('',*,*,#1649,.T.);
#2120=ORIENTED_EDGE('',*,*,#1647,.F.);
#2121=ORIENTED_EDGE('',*,*,#1650,.T.);
#2122=ORIENTED_EDGE('',*,*,#1651,.T.);
#2123=ORIENTED_EDGE('',*,*,#1652,.F.);
#2124=ORIENTED_EDGE('',*,*,#1653,.T.);
#2125=ORIENTED_EDGE('',*,*,#1654,.T.);
#2126=ORIENTED_EDGE('',*,*,#1655,.T.);
#2127=ORIENTED_EDGE('',*,*,#1656,.T.);
#2128=ORIENTED_EDGE('',*,*,#1654,.F.);
#2129=ORIENTED_EDGE('',*,*,#1657,.F.);
#2130=ORIENTED_EDGE('',*,*,#1658,.F.);
#2131=ORIENTED_EDGE('',*,*,#1659,.F.);
#2132=ORIENTED_EDGE('',*,*,#1660,.T.);
#2133=ORIENTED_EDGE('',*,*,#1661,.T.);
#2134=ORIENTED_EDGE('',*,*,#1662,.T.);
#2135=ORIENTED_EDGE('',*,*,#1663,.T.);
#2136=ORIENTED_EDGE('',*,*,#1661,.F.);
#2137=ORIENTED_EDGE('',*,*,#1664,.T.);
#2138=ORIENTED_EDGE('',*,*,#1665,.T.);
#2139=ORIENTED_EDGE('',*,*,#1666,.F.);
#2140=ORIENTED_EDGE('',*,*,#1667,.T.);
#2141=ORIENTED_EDGE('',*,*,#1668,.T.);
#2142=ORIENTED_EDGE('',*,*,#1669,.T.);
#2143=ORIENTED_EDGE('',*,*,#1670,.T.);
#2144=ORIENTED_EDGE('',*,*,#1668,.F.);
#2145=ORIENTED_EDGE('',*,*,#1671,.F.);
#2146=ORIENTED_EDGE('',*,*,#1672,.F.);
#2147=ORIENTED_EDGE('',*,*,#1673,.F.);
#2148=ORIENTED_EDGE('',*,*,#1674,.T.);
#2149=ORIENTED_EDGE('',*,*,#1675,.T.);
#2150=ORIENTED_EDGE('',*,*,#1676,.T.);
#2151=ORIENTED_EDGE('',*,*,#1677,.T.);
#2152=ORIENTED_EDGE('',*,*,#1675,.F.);
#2153=ORIENTED_EDGE('',*,*,#1678,.T.);
#2154=ORIENTED_EDGE('',*,*,#1679,.T.);
#2155=ORIENTED_EDGE('',*,*,#1680,.F.);
#2156=ORIENTED_EDGE('',*,*,#1681,.T.);
#2157=ORIENTED_EDGE('',*,*,#1682,.T.);
#2158=ORIENTED_EDGE('',*,*,#1683,.T.);
#2159=ORIENTED_EDGE('',*,*,#1684,.T.);
#2160=ORIENTED_EDGE('',*,*,#1682,.F.);
#2161=ORIENTED_EDGE('',*,*,#1685,.F.);
#2162=ORIENTED_EDGE('',*,*,#1686,.F.);
#2163=ORIENTED_EDGE('',*,*,#1687,.F.);
#2164=ORIENTED_EDGE('',*,*,#1688,.T.);
#2165=ORIENTED_EDGE('',*,*,#1689,.T.);
#2166=ORIENTED_EDGE('',*,*,#1690,.T.);
#2167=ORIENTED_EDGE('',*,*,#1691,.T.);
#2168=ORIENTED_EDGE('',*,*,#1689,.F.);
#2169=ORIENTED_EDGE('',*,*,#1692,.T.);
#2170=ORIENTED_EDGE('',*,*,#1693,.T.);
#2171=ORIENTED_EDGE('',*,*,#1694,.F.);
#2172=ORIENTED_EDGE('',*,*,#1695,.F.);
#2173=ORIENTED_EDGE('',*,*,#1630,.T.);
#2174=ORIENTED_EDGE('',*,*,#1696,.F.);
#2175=ORIENTED_EDGE('',*,*,#1697,.F.);
#2176=ORIENTED_EDGE('',*,*,#1698,.T.);
#2177=ORIENTED_EDGE('',*,*,#1697,.T.);
#2178=ORIENTED_EDGE('',*,*,#1699,.F.);
#2179=ORIENTED_EDGE('',*,*,#1700,.F.);
#2180=ORIENTED_EDGE('',*,*,#1701,.T.);
#2181=ORIENTED_EDGE('',*,*,#1700,.T.);
#2182=ORIENTED_EDGE('',*,*,#1702,.F.);
#2183=ORIENTED_EDGE('',*,*,#1637,.F.);
#2184=ORIENTED_EDGE('',*,*,#1703,.F.);
#2185=ORIENTED_EDGE('',*,*,#1644,.T.);
#2186=ORIENTED_EDGE('',*,*,#1704,.F.);
#2187=ORIENTED_EDGE('',*,*,#1705,.F.);
#2188=ORIENTED_EDGE('',*,*,#1706,.T.);
#2189=ORIENTED_EDGE('',*,*,#1705,.T.);
#2190=ORIENTED_EDGE('',*,*,#1707,.F.);
#2191=ORIENTED_EDGE('',*,*,#1708,.F.);
#2192=ORIENTED_EDGE('',*,*,#1709,.T.);
#2193=ORIENTED_EDGE('',*,*,#1708,.T.);
#2194=ORIENTED_EDGE('',*,*,#1710,.F.);
#2195=ORIENTED_EDGE('',*,*,#1651,.F.);
#2196=ORIENTED_EDGE('',*,*,#1711,.F.);
#2197=ORIENTED_EDGE('',*,*,#1658,.T.);
#2198=ORIENTED_EDGE('',*,*,#1712,.F.);
#2199=ORIENTED_EDGE('',*,*,#1713,.F.);
#2200=ORIENTED_EDGE('',*,*,#1714,.T.);
#2201=ORIENTED_EDGE('',*,*,#1713,.T.);
#2202=ORIENTED_EDGE('',*,*,#1715,.F.);
#2203=ORIENTED_EDGE('',*,*,#1716,.F.);
#2204=ORIENTED_EDGE('',*,*,#1717,.T.);
#2205=ORIENTED_EDGE('',*,*,#1716,.T.);
#2206=ORIENTED_EDGE('',*,*,#1718,.F.);
#2207=ORIENTED_EDGE('',*,*,#1665,.F.);
#2208=ORIENTED_EDGE('',*,*,#1719,.F.);
#2209=ORIENTED_EDGE('',*,*,#1672,.T.);
#2210=ORIENTED_EDGE('',*,*,#1720,.F.);
#2211=ORIENTED_EDGE('',*,*,#1721,.F.);
#2212=ORIENTED_EDGE('',*,*,#1722,.T.);
#2213=ORIENTED_EDGE('',*,*,#1721,.T.);
#2214=ORIENTED_EDGE('',*,*,#1723,.F.);
#2215=ORIENTED_EDGE('',*,*,#1724,.F.);
#2216=ORIENTED_EDGE('',*,*,#1725,.T.);
#2217=ORIENTED_EDGE('',*,*,#1724,.T.);
#2218=ORIENTED_EDGE('',*,*,#1726,.F.);
#2219=ORIENTED_EDGE('',*,*,#1679,.F.);
#2220=ORIENTED_EDGE('',*,*,#1727,.F.);
#2221=ORIENTED_EDGE('',*,*,#1686,.T.);
#2222=ORIENTED_EDGE('',*,*,#1728,.F.);
#2223=ORIENTED_EDGE('',*,*,#1729,.F.);
#2224=ORIENTED_EDGE('',*,*,#1730,.T.);
#2225=ORIENTED_EDGE('',*,*,#1729,.T.);
#2226=ORIENTED_EDGE('',*,*,#1731,.F.);
#2227=ORIENTED_EDGE('',*,*,#1732,.F.);
#2228=ORIENTED_EDGE('',*,*,#1733,.T.);
#2229=ORIENTED_EDGE('',*,*,#1732,.T.);
#2230=ORIENTED_EDGE('',*,*,#1734,.F.);
#2231=ORIENTED_EDGE('',*,*,#1693,.F.);
#2232=ORIENTED_EDGE('',*,*,#1641,.F.);
#2233=ORIENTED_EDGE('',*,*,#1645,.T.);
#2234=ORIENTED_EDGE('',*,*,#1703,.T.);
#2235=ORIENTED_EDGE('',*,*,#1706,.F.);
#2236=ORIENTED_EDGE('',*,*,#1709,.F.);
#2237=ORIENTED_EDGE('',*,*,#1650,.F.);
#2238=ORIENTED_EDGE('',*,*,#1646,.F.);
#2239=ORIENTED_EDGE('',*,*,#1735,.F.);
#2240=ORIENTED_EDGE('',*,*,#1655,.F.);
#2241=ORIENTED_EDGE('',*,*,#1659,.T.);
#2242=ORIENTED_EDGE('',*,*,#1711,.T.);
#2243=ORIENTED_EDGE('',*,*,#1714,.F.);
#2244=ORIENTED_EDGE('',*,*,#1717,.F.);
#2245=ORIENTED_EDGE('',*,*,#1664,.F.);
#2246=ORIENTED_EDGE('',*,*,#1660,.F.);
#2247=ORIENTED_EDGE('',*,*,#1736,.F.);
#2248=ORIENTED_EDGE('',*,*,#1669,.F.);
#2249=ORIENTED_EDGE('',*,*,#1673,.T.);
#2250=ORIENTED_EDGE('',*,*,#1719,.T.);
#2251=ORIENTED_EDGE('',*,*,#1722,.F.);
#2252=ORIENTED_EDGE('',*,*,#1725,.F.);
#2253=ORIENTED_EDGE('',*,*,#1678,.F.);
#2254=ORIENTED_EDGE('',*,*,#1674,.F.);
#2255=ORIENTED_EDGE('',*,*,#1737,.F.);
#2256=ORIENTED_EDGE('',*,*,#1683,.F.);
#2257=ORIENTED_EDGE('',*,*,#1687,.T.);
#2258=ORIENTED_EDGE('',*,*,#1727,.T.);
#2259=ORIENTED_EDGE('',*,*,#1730,.F.);
#2260=ORIENTED_EDGE('',*,*,#1733,.F.);
#2261=ORIENTED_EDGE('',*,*,#1692,.F.);
#2262=ORIENTED_EDGE('',*,*,#1688,.F.);
#2263=ORIENTED_EDGE('',*,*,#1738,.F.);
#2264=ORIENTED_EDGE('',*,*,#1739,.F.);
#2265=ORIENTED_EDGE('',*,*,#1740,.T.);
#2266=ORIENTED_EDGE('',*,*,#1741,.T.);
#2267=ORIENTED_EDGE('',*,*,#1742,.F.);
#2268=ORIENTED_EDGE('',*,*,#1743,.F.);
#2269=ORIENTED_EDGE('',*,*,#1744,.F.);
#2270=ORIENTED_EDGE('',*,*,#1745,.F.);
#2271=ORIENTED_EDGE('',*,*,#1746,.F.);
#2272=ORIENTED_EDGE('',*,*,#1627,.F.);
#2273=ORIENTED_EDGE('',*,*,#1631,.T.);
#2274=ORIENTED_EDGE('',*,*,#1695,.T.);
#2275=ORIENTED_EDGE('',*,*,#1698,.F.);
#2276=ORIENTED_EDGE('',*,*,#1701,.F.);
#2277=ORIENTED_EDGE('',*,*,#1636,.F.);
#2278=ORIENTED_EDGE('',*,*,#1632,.F.);
#2279=ORIENTED_EDGE('',*,*,#1747,.F.);
#2280=ORIENTED_EDGE('',*,*,#1748,.F.);
#2281=ORIENTED_EDGE('',*,*,#1691,.F.);
#2282=ORIENTED_EDGE('',*,*,#1749,.F.);
#2283=ORIENTED_EDGE('',*,*,#1750,.F.);
#2284=ORIENTED_EDGE('',*,*,#1738,.T.);
#2285=ORIENTED_EDGE('',*,*,#1677,.F.);
#2286=ORIENTED_EDGE('',*,*,#1751,.F.);
#2287=ORIENTED_EDGE('',*,*,#1684,.F.);
#2288=ORIENTED_EDGE('',*,*,#1737,.T.);
#2289=ORIENTED_EDGE('',*,*,#1663,.F.);
#2290=ORIENTED_EDGE('',*,*,#1752,.F.);
#2291=ORIENTED_EDGE('',*,*,#1670,.F.);
#2292=ORIENTED_EDGE('',*,*,#1736,.T.);
#2293=ORIENTED_EDGE('',*,*,#1649,.F.);
#2294=ORIENTED_EDGE('',*,*,#1753,.F.);
#2295=ORIENTED_EDGE('',*,*,#1656,.F.);
#2296=ORIENTED_EDGE('',*,*,#1735,.T.);
#2297=ORIENTED_EDGE('',*,*,#1635,.F.);
#2298=ORIENTED_EDGE('',*,*,#1754,.F.);
#2299=ORIENTED_EDGE('',*,*,#1642,.F.);
#2300=ORIENTED_EDGE('',*,*,#1747,.T.);
#2301=ORIENTED_EDGE('',*,*,#1755,.T.);
#2302=ORIENTED_EDGE('',*,*,#1756,.T.);
#2303=ORIENTED_EDGE('',*,*,#1739,.T.);
#2304=ORIENTED_EDGE('',*,*,#1750,.T.);
#2305=ORIENTED_EDGE('',*,*,#1756,.F.);
#2306=ORIENTED_EDGE('',*,*,#1757,.F.);
#2307=ORIENTED_EDGE('',*,*,#1758,.F.);
#2308=ORIENTED_EDGE('',*,*,#1740,.F.);
#2309=ORIENTED_EDGE('',*,*,#1745,.T.);
#2310=ORIENTED_EDGE('',*,*,#1759,.T.);
#2311=ORIENTED_EDGE('',*,*,#1760,.T.);
#2312=ORIENTED_EDGE('',*,*,#1761,.T.);
#2313=ORIENTED_EDGE('',*,*,#1759,.F.);
#2314=ORIENTED_EDGE('',*,*,#1744,.T.);
#2315=ORIENTED_EDGE('',*,*,#1762,.T.);
#2316=ORIENTED_EDGE('',*,*,#1763,.F.);
#2317=ORIENTED_EDGE('',*,*,#1741,.F.);
#2318=ORIENTED_EDGE('',*,*,#1758,.T.);
#2319=ORIENTED_EDGE('',*,*,#1764,.F.);
#2320=ORIENTED_EDGE('',*,*,#1765,.F.);
#2321=ORIENTED_EDGE('',*,*,#1742,.T.);
#2322=ORIENTED_EDGE('',*,*,#1765,.T.);
#2323=ORIENTED_EDGE('',*,*,#1766,.F.);
#2324=ORIENTED_EDGE('',*,*,#1767,.F.);
#2325=ORIENTED_EDGE('',*,*,#1743,.T.);
#2326=ORIENTED_EDGE('',*,*,#1767,.T.);
#2327=ORIENTED_EDGE('',*,*,#1768,.F.);
#2328=ORIENTED_EDGE('',*,*,#1762,.F.);
#2329=ORIENTED_EDGE('',*,*,#1769,.T.);
#2330=ORIENTED_EDGE('',*,*,#1760,.F.);
#2331=ORIENTED_EDGE('',*,*,#1763,.T.);
#2332=ORIENTED_EDGE('',*,*,#1768,.T.);
#2333=ORIENTED_EDGE('',*,*,#1766,.T.);
#2334=ORIENTED_EDGE('',*,*,#1764,.T.);
#2335=ORIENTED_EDGE('',*,*,#1757,.T.);
#2336=ORIENTED_EDGE('',*,*,#1755,.F.);
#2337=ORIENTED_EDGE('',*,*,#1749,.T.);
#2338=ORIENTED_EDGE('',*,*,#1690,.F.);
#2339=ORIENTED_EDGE('',*,*,#1694,.T.);
#2340=ORIENTED_EDGE('',*,*,#1734,.T.);
#2341=ORIENTED_EDGE('',*,*,#1731,.T.);
#2342=ORIENTED_EDGE('',*,*,#1728,.T.);
#2343=ORIENTED_EDGE('',*,*,#1685,.T.);
#2344=ORIENTED_EDGE('',*,*,#1681,.F.);
#2345=ORIENTED_EDGE('',*,*,#1751,.T.);
#2346=ORIENTED_EDGE('',*,*,#1676,.F.);
#2347=ORIENTED_EDGE('',*,*,#1680,.T.);
#2348=ORIENTED_EDGE('',*,*,#1726,.T.);
#2349=ORIENTED_EDGE('',*,*,#1723,.T.);
#2350=ORIENTED_EDGE('',*,*,#1720,.T.);
#2351=ORIENTED_EDGE('',*,*,#1671,.T.);
#2352=ORIENTED_EDGE('',*,*,#1667,.F.);
#2353=ORIENTED_EDGE('',*,*,#1752,.T.);
#2354=ORIENTED_EDGE('',*,*,#1662,.F.);
#2355=ORIENTED_EDGE('',*,*,#1666,.T.);
#2356=ORIENTED_EDGE('',*,*,#1718,.T.);
#2357=ORIENTED_EDGE('',*,*,#1715,.T.);
#2358=ORIENTED_EDGE('',*,*,#1712,.T.);
#2359=ORIENTED_EDGE('',*,*,#1657,.T.);
#2360=ORIENTED_EDGE('',*,*,#1653,.F.);
#2361=ORIENTED_EDGE('',*,*,#1753,.T.);
#2362=ORIENTED_EDGE('',*,*,#1648,.F.);
#2363=ORIENTED_EDGE('',*,*,#1652,.T.);
#2364=ORIENTED_EDGE('',*,*,#1710,.T.);
#2365=ORIENTED_EDGE('',*,*,#1707,.T.);
#2366=ORIENTED_EDGE('',*,*,#1704,.T.);
#2367=ORIENTED_EDGE('',*,*,#1643,.T.);
#2368=ORIENTED_EDGE('',*,*,#1639,.F.);
#2369=ORIENTED_EDGE('',*,*,#1754,.T.);
#2370=ORIENTED_EDGE('',*,*,#1634,.F.);
#2371=ORIENTED_EDGE('',*,*,#1638,.T.);
#2372=ORIENTED_EDGE('',*,*,#1702,.T.);
#2373=ORIENTED_EDGE('',*,*,#1699,.T.);
#2374=ORIENTED_EDGE('',*,*,#1696,.T.);
#2375=ORIENTED_EDGE('',*,*,#1629,.T.);
#2376=ORIENTED_EDGE('',*,*,#1625,.F.);
#2377=ORIENTED_EDGE('',*,*,#1770,.T.);
#2378=ORIENTED_EDGE('',*,*,#1748,.T.);
#2379=ORIENTED_EDGE('',*,*,#1771,.T.);
#2380=ORIENTED_EDGE('',*,*,#1770,.F.);
#2381=ORIENTED_EDGE('',*,*,#1771,.F.);
#2382=ORIENTED_EDGE('',*,*,#1628,.F.);
#2383=ORIENTED_EDGE('',*,*,#1746,.T.);
#2384=ORIENTED_EDGE('',*,*,#1761,.F.);
#2385=ORIENTED_EDGE('',*,*,#1769,.F.);
#2386=ORIENTED_EDGE('',*,*,#1772,.F.);
#2387=ORIENTED_EDGE('',*,*,#1773,.F.);
#2388=ORIENTED_EDGE('',*,*,#1774,.T.);
#2389=ORIENTED_EDGE('',*,*,#1775,.F.);
#2390=ORIENTED_EDGE('',*,*,#1776,.F.);
#2391=ORIENTED_EDGE('',*,*,#1774,.F.);
#2392=ORIENTED_EDGE('',*,*,#1773,.T.);
#2393=ORIENTED_EDGE('',*,*,#1777,.F.);
#2394=ORIENTED_EDGE('',*,*,#1778,.F.);
#2395=ORIENTED_EDGE('',*,*,#1779,.F.);
#2396=ORIENTED_EDGE('',*,*,#1772,.T.);
#2397=ORIENTED_EDGE('',*,*,#1780,.F.);
#2398=ORIENTED_EDGE('',*,*,#1781,.F.);
#2399=ORIENTED_EDGE('',*,*,#1782,.F.);
#2400=ORIENTED_EDGE('',*,*,#1783,.F.);
#2401=ORIENTED_EDGE('',*,*,#1784,.T.);
#2402=ORIENTED_EDGE('',*,*,#1778,.T.);
#2403=ORIENTED_EDGE('',*,*,#1785,.F.);
#2404=ORIENTED_EDGE('',*,*,#1786,.F.);
#2405=ORIENTED_EDGE('',*,*,#1785,.T.);
#2406=ORIENTED_EDGE('',*,*,#1777,.T.);
#2407=ORIENTED_EDGE('',*,*,#1782,.T.);
#2408=ORIENTED_EDGE('',*,*,#1787,.F.);
#2409=ORIENTED_EDGE('',*,*,#1788,.F.);
#2410=ORIENTED_EDGE('',*,*,#1789,.F.);
#2411=ORIENTED_EDGE('',*,*,#1780,.T.);
#2412=ORIENTED_EDGE('',*,*,#1779,.T.);
#2413=ORIENTED_EDGE('',*,*,#1784,.F.);
#2414=ORIENTED_EDGE('',*,*,#1790,.T.);
#2415=ORIENTED_EDGE('',*,*,#1791,.T.);
#2416=ORIENTED_EDGE('',*,*,#1792,.F.);
#2417=ORIENTED_EDGE('',*,*,#1788,.T.);
#2418=ORIENTED_EDGE('',*,*,#1783,.T.);
#2419=ORIENTED_EDGE('',*,*,#1786,.T.);
#2420=ORIENTED_EDGE('',*,*,#1793,.F.);
#2421=ORIENTED_EDGE('',*,*,#1791,.F.);
#2422=ORIENTED_EDGE('',*,*,#1794,.F.);
#2423=ORIENTED_EDGE('',*,*,#1795,.F.);
#2424=ORIENTED_EDGE('',*,*,#1796,.T.);
#2425=ORIENTED_EDGE('',*,*,#1797,.F.);
#2426=ORIENTED_EDGE('',*,*,#1798,.T.);
#2427=ORIENTED_EDGE('',*,*,#1799,.F.);
#2428=ORIENTED_EDGE('',*,*,#1800,.F.);
#2429=ORIENTED_EDGE('',*,*,#1801,.F.);
#2430=ORIENTED_EDGE('',*,*,#1802,.T.);
#2431=ORIENTED_EDGE('',*,*,#1803,.F.);
#2432=ORIENTED_EDGE('',*,*,#1804,.F.);
#2433=ORIENTED_EDGE('',*,*,#1805,.F.);
#2434=ORIENTED_EDGE('',*,*,#1806,.T.);
#2435=ORIENTED_EDGE('',*,*,#1807,.F.);
#2436=ORIENTED_EDGE('',*,*,#1803,.T.);
#2437=ORIENTED_EDGE('',*,*,#1808,.F.);
#2438=ORIENTED_EDGE('',*,*,#1797,.T.);
#2439=ORIENTED_EDGE('',*,*,#1809,.F.);
#2440=ORIENTED_EDGE('',*,*,#1799,.T.);
#2441=ORIENTED_EDGE('',*,*,#1807,.T.);
#2442=ORIENTED_EDGE('',*,*,#1810,.T.);
#2443=ORIENTED_EDGE('',*,*,#1811,.F.);
#2444=ORIENTED_EDGE('',*,*,#1812,.F.);
#2445=ORIENTED_EDGE('',*,*,#1809,.T.);
#2446=ORIENTED_EDGE('',*,*,#1813,.T.);
#2447=ORIENTED_EDGE('',*,*,#1814,.F.);
#2448=ORIENTED_EDGE('',*,*,#1815,.F.);
#2449=ORIENTED_EDGE('',*,*,#1805,.T.);
#2450=ORIENTED_EDGE('',*,*,#1816,.F.);
#2451=ORIENTED_EDGE('',*,*,#1817,.F.);
#2452=ORIENTED_EDGE('',*,*,#1818,.T.);
#2453=ORIENTED_EDGE('',*,*,#1819,.F.);
#2454=ORIENTED_EDGE('',*,*,#1820,.T.);
#2455=ORIENTED_EDGE('',*,*,#1821,.F.);
#2456=ORIENTED_EDGE('',*,*,#1822,.F.);
#2457=ORIENTED_EDGE('',*,*,#1801,.T.);
#2458=ORIENTED_EDGE('',*,*,#1823,.F.);
#2459=ORIENTED_EDGE('',*,*,#1824,.F.);
#2460=ORIENTED_EDGE('',*,*,#1825,.T.);
#2461=ORIENTED_EDGE('',*,*,#1826,.F.);
#2462=ORIENTED_EDGE('',*,*,#1827,.T.);
#2463=ORIENTED_EDGE('',*,*,#1828,.F.);
#2464=ORIENTED_EDGE('',*,*,#1829,.F.);
#2465=ORIENTED_EDGE('',*,*,#1795,.T.);
#2466=ORIENTED_EDGE('',*,*,#1830,.F.);
#2467=ORIENTED_EDGE('',*,*,#1831,.F.);
#2468=ORIENTED_EDGE('',*,*,#1832,.T.);
#2469=ORIENTED_EDGE('',*,*,#1833,.F.);
#2470=ORIENTED_EDGE('',*,*,#1834,.T.);
#2471=ORIENTED_EDGE('',*,*,#1835,.F.);
#2472=ORIENTED_EDGE('',*,*,#1836,.F.);
#2473=ORIENTED_EDGE('',*,*,#1790,.F.);
#2474=ORIENTED_EDGE('',*,*,#1837,.F.);
#2475=ORIENTED_EDGE('',*,*,#1838,.T.);
#2476=ORIENTED_EDGE('',*,*,#1839,.F.);
#2477=ORIENTED_EDGE('',*,*,#1838,.F.);
#2478=ORIENTED_EDGE('',*,*,#1775,.T.);
#2479=ORIENTED_EDGE('',*,*,#1776,.T.);
#2480=ORIENTED_EDGE('',*,*,#1837,.T.);
#2481=ORIENTED_EDGE('',*,*,#1789,.T.);
#2482=ORIENTED_EDGE('',*,*,#1792,.T.);
#2483=ORIENTED_EDGE('',*,*,#1793,.T.);
#2484=ORIENTED_EDGE('',*,*,#1787,.T.);
#2485=ORIENTED_EDGE('',*,*,#1781,.T.);
#2486=ORIENTED_EDGE('',*,*,#1840,.F.);
#2487=ORIENTED_EDGE('',*,*,#1841,.T.);
#2488=ORIENTED_EDGE('',*,*,#1806,.F.);
#2489=ORIENTED_EDGE('',*,*,#1841,.F.);
#2490=ORIENTED_EDGE('',*,*,#1840,.T.);
#2491=ORIENTED_EDGE('',*,*,#1839,.T.);
#2492=ORIENTED_EDGE('',*,*,#1819,.T.);
#2493=ORIENTED_EDGE('',*,*,#1842,.T.);
#2494=ORIENTED_EDGE('',*,*,#1843,.F.);
#2495=ORIENTED_EDGE('',*,*,#1844,.F.);
#2496=ORIENTED_EDGE('',*,*,#1820,.F.);
#2497=ORIENTED_EDGE('',*,*,#1844,.T.);
#2498=ORIENTED_EDGE('',*,*,#1845,.F.);
#2499=ORIENTED_EDGE('',*,*,#1846,.F.);
#2500=ORIENTED_EDGE('',*,*,#1821,.T.);
#2501=ORIENTED_EDGE('',*,*,#1846,.T.);
#2502=ORIENTED_EDGE('',*,*,#1847,.F.);
#2503=ORIENTED_EDGE('',*,*,#1848,.F.);
#2504=ORIENTED_EDGE('',*,*,#1822,.T.);
#2505=ORIENTED_EDGE('',*,*,#1848,.T.);
#2506=ORIENTED_EDGE('',*,*,#1849,.F.);
#2507=ORIENTED_EDGE('',*,*,#1810,.F.);
#2508=ORIENTED_EDGE('',*,*,#1798,.F.);
#2509=ORIENTED_EDGE('',*,*,#1816,.T.);
#2510=ORIENTED_EDGE('',*,*,#1804,.T.);
#2511=ORIENTED_EDGE('',*,*,#1812,.T.);
#2512=ORIENTED_EDGE('',*,*,#1850,.F.);
#2513=ORIENTED_EDGE('',*,*,#1851,.F.);
#2514=ORIENTED_EDGE('',*,*,#1817,.T.);
#2515=ORIENTED_EDGE('',*,*,#1851,.T.);
#2516=ORIENTED_EDGE('',*,*,#1852,.F.);
#2517=ORIENTED_EDGE('',*,*,#1853,.F.);
#2518=ORIENTED_EDGE('',*,*,#1818,.F.);
#2519=ORIENTED_EDGE('',*,*,#1853,.T.);
#2520=ORIENTED_EDGE('',*,*,#1854,.F.);
#2521=ORIENTED_EDGE('',*,*,#1842,.F.);
#2522=ORIENTED_EDGE('',*,*,#1854,.T.);
#2523=ORIENTED_EDGE('',*,*,#1852,.T.);
#2524=ORIENTED_EDGE('',*,*,#1850,.T.);
#2525=ORIENTED_EDGE('',*,*,#1811,.T.);
#2526=ORIENTED_EDGE('',*,*,#1849,.T.);
#2527=ORIENTED_EDGE('',*,*,#1847,.T.);
#2528=ORIENTED_EDGE('',*,*,#1845,.T.);
#2529=ORIENTED_EDGE('',*,*,#1843,.T.);
#2530=ORIENTED_EDGE('',*,*,#1826,.T.);
#2531=ORIENTED_EDGE('',*,*,#1855,.T.);
#2532=ORIENTED_EDGE('',*,*,#1856,.F.);
#2533=ORIENTED_EDGE('',*,*,#1857,.F.);
#2534=ORIENTED_EDGE('',*,*,#1827,.F.);
#2535=ORIENTED_EDGE('',*,*,#1857,.T.);
#2536=ORIENTED_EDGE('',*,*,#1858,.F.);
#2537=ORIENTED_EDGE('',*,*,#1859,.F.);
#2538=ORIENTED_EDGE('',*,*,#1828,.T.);
#2539=ORIENTED_EDGE('',*,*,#1859,.T.);
#2540=ORIENTED_EDGE('',*,*,#1860,.F.);
#2541=ORIENTED_EDGE('',*,*,#1861,.F.);
#2542=ORIENTED_EDGE('',*,*,#1829,.T.);
#2543=ORIENTED_EDGE('',*,*,#1861,.T.);
#2544=ORIENTED_EDGE('',*,*,#1862,.F.);
#2545=ORIENTED_EDGE('',*,*,#1813,.F.);
#2546=ORIENTED_EDGE('',*,*,#1796,.F.);
#2547=ORIENTED_EDGE('',*,*,#1823,.T.);
#2548=ORIENTED_EDGE('',*,*,#1800,.T.);
#2549=ORIENTED_EDGE('',*,*,#1815,.T.);
#2550=ORIENTED_EDGE('',*,*,#1863,.F.);
#2551=ORIENTED_EDGE('',*,*,#1864,.F.);
#2552=ORIENTED_EDGE('',*,*,#1824,.T.);
#2553=ORIENTED_EDGE('',*,*,#1864,.T.);
#2554=ORIENTED_EDGE('',*,*,#1865,.F.);
#2555=ORIENTED_EDGE('',*,*,#1866,.F.);
#2556=ORIENTED_EDGE('',*,*,#1825,.F.);
#2557=ORIENTED_EDGE('',*,*,#1866,.T.);
#2558=ORIENTED_EDGE('',*,*,#1867,.F.);
#2559=ORIENTED_EDGE('',*,*,#1855,.F.);
#2560=ORIENTED_EDGE('',*,*,#1867,.T.);
#2561=ORIENTED_EDGE('',*,*,#1865,.T.);
#2562=ORIENTED_EDGE('',*,*,#1863,.T.);
#2563=ORIENTED_EDGE('',*,*,#1814,.T.);
#2564=ORIENTED_EDGE('',*,*,#1862,.T.);
#2565=ORIENTED_EDGE('',*,*,#1860,.T.);
#2566=ORIENTED_EDGE('',*,*,#1858,.T.);
#2567=ORIENTED_EDGE('',*,*,#1856,.T.);
#2568=ORIENTED_EDGE('',*,*,#1833,.T.);
#2569=ORIENTED_EDGE('',*,*,#1868,.T.);
#2570=ORIENTED_EDGE('',*,*,#1869,.F.);
#2571=ORIENTED_EDGE('',*,*,#1870,.F.);
#2572=ORIENTED_EDGE('',*,*,#1834,.F.);
#2573=ORIENTED_EDGE('',*,*,#1870,.T.);
#2574=ORIENTED_EDGE('',*,*,#1871,.F.);
#2575=ORIENTED_EDGE('',*,*,#1872,.F.);
#2576=ORIENTED_EDGE('',*,*,#1835,.T.);
#2577=ORIENTED_EDGE('',*,*,#1872,.T.);
#2578=ORIENTED_EDGE('',*,*,#1873,.F.);
#2579=ORIENTED_EDGE('',*,*,#1874,.F.);
#2580=ORIENTED_EDGE('',*,*,#1836,.T.);
#2581=ORIENTED_EDGE('',*,*,#1874,.T.);
#2582=ORIENTED_EDGE('',*,*,#1875,.F.);
#2583=ORIENTED_EDGE('',*,*,#1876,.F.);
#2584=ORIENTED_EDGE('',*,*,#1802,.F.);
#2585=ORIENTED_EDGE('',*,*,#1808,.T.);
#2586=ORIENTED_EDGE('',*,*,#1876,.T.);
#2587=ORIENTED_EDGE('',*,*,#1877,.F.);
#2588=ORIENTED_EDGE('',*,*,#1878,.F.);
#2589=ORIENTED_EDGE('',*,*,#1830,.T.);
#2590=ORIENTED_EDGE('',*,*,#1794,.T.);
#2591=ORIENTED_EDGE('',*,*,#1878,.T.);
#2592=ORIENTED_EDGE('',*,*,#1879,.F.);
#2593=ORIENTED_EDGE('',*,*,#1880,.F.);
#2594=ORIENTED_EDGE('',*,*,#1831,.T.);
#2595=ORIENTED_EDGE('',*,*,#1880,.T.);
#2596=ORIENTED_EDGE('',*,*,#1881,.F.);
#2597=ORIENTED_EDGE('',*,*,#1882,.F.);
#2598=ORIENTED_EDGE('',*,*,#1832,.F.);
#2599=ORIENTED_EDGE('',*,*,#1882,.T.);
#2600=ORIENTED_EDGE('',*,*,#1883,.F.);
#2601=ORIENTED_EDGE('',*,*,#1868,.F.);
#2602=ORIENTED_EDGE('',*,*,#1883,.T.);
#2603=ORIENTED_EDGE('',*,*,#1881,.T.);
#2604=ORIENTED_EDGE('',*,*,#1879,.T.);
#2605=ORIENTED_EDGE('',*,*,#1877,.T.);
#2606=ORIENTED_EDGE('',*,*,#1875,.T.);
#2607=ORIENTED_EDGE('',*,*,#1873,.T.);
#2608=ORIENTED_EDGE('',*,*,#1871,.T.);
#2609=ORIENTED_EDGE('',*,*,#1869,.T.);
#2610=ORIENTED_EDGE('',*,*,#1884,.F.);
#2611=ORIENTED_EDGE('',*,*,#1885,.F.);
#2612=ORIENTED_EDGE('',*,*,#1886,.T.);
#2613=ORIENTED_EDGE('',*,*,#1887,.F.);
#2614=ORIENTED_EDGE('',*,*,#1888,.F.);
#2615=ORIENTED_EDGE('',*,*,#1886,.F.);
#2616=ORIENTED_EDGE('',*,*,#1885,.T.);
#2617=ORIENTED_EDGE('',*,*,#1889,.T.);
#2618=ORIENTED_EDGE('',*,*,#1890,.F.);
#2619=ORIENTED_EDGE('',*,*,#1891,.T.);
#2620=ORIENTED_EDGE('',*,*,#1884,.T.);
#2621=ORIENTED_EDGE('',*,*,#1892,.T.);
#2622=ORIENTED_EDGE('',*,*,#1893,.T.);
#2623=ORIENTED_EDGE('',*,*,#1894,.T.);
#2624=ORIENTED_EDGE('',*,*,#1895,.F.);
#2625=ORIENTED_EDGE('',*,*,#1889,.F.);
#2626=ORIENTED_EDGE('',*,*,#1894,.F.);
#2627=ORIENTED_EDGE('',*,*,#1896,.F.);
#2628=ORIENTED_EDGE('',*,*,#1897,.F.);
#2629=ORIENTED_EDGE('',*,*,#1898,.F.);
#2630=ORIENTED_EDGE('',*,*,#1896,.T.);
#2631=ORIENTED_EDGE('',*,*,#1893,.F.);
#2632=ORIENTED_EDGE('',*,*,#1899,.F.);
#2633=ORIENTED_EDGE('',*,*,#1900,.F.);
#2634=ORIENTED_EDGE('',*,*,#1901,.F.);
#2635=ORIENTED_EDGE('',*,*,#1899,.T.);
#2636=ORIENTED_EDGE('',*,*,#1892,.F.);
#2637=ORIENTED_EDGE('',*,*,#1891,.F.);
#2638=ORIENTED_EDGE('',*,*,#1902,.T.);
#2639=ORIENTED_EDGE('',*,*,#1903,.T.);
#2640=ORIENTED_EDGE('',*,*,#1904,.F.);
#2641=ORIENTED_EDGE('',*,*,#1903,.F.);
#2642=ORIENTED_EDGE('',*,*,#1905,.T.);
#2643=ORIENTED_EDGE('',*,*,#1897,.T.);
#2644=ORIENTED_EDGE('',*,*,#1898,.T.);
#2645=ORIENTED_EDGE('',*,*,#1901,.T.);
#2646=ORIENTED_EDGE('',*,*,#1906,.T.);
#2647=ORIENTED_EDGE('',*,*,#1907,.T.);
#2648=ORIENTED_EDGE('',*,*,#1908,.F.);
#2649=ORIENTED_EDGE('',*,*,#1909,.T.);
#2650=ORIENTED_EDGE('',*,*,#1910,.F.);
#2651=ORIENTED_EDGE('',*,*,#1911,.T.);
#2652=ORIENTED_EDGE('',*,*,#1912,.T.);
#2653=ORIENTED_EDGE('',*,*,#1913,.T.);
#2654=ORIENTED_EDGE('',*,*,#1914,.F.);
#2655=ORIENTED_EDGE('',*,*,#1915,.T.);
#2656=ORIENTED_EDGE('',*,*,#1916,.T.);
#2657=ORIENTED_EDGE('',*,*,#1917,.T.);
#2658=ORIENTED_EDGE('',*,*,#1918,.F.);
#2659=ORIENTED_EDGE('',*,*,#1919,.T.);
#2660=ORIENTED_EDGE('',*,*,#1913,.F.);
#2661=ORIENTED_EDGE('',*,*,#1920,.T.);
#2662=ORIENTED_EDGE('',*,*,#1907,.F.);
#2663=ORIENTED_EDGE('',*,*,#1921,.T.);
#2664=ORIENTED_EDGE('',*,*,#1917,.F.);
#2665=ORIENTED_EDGE('',*,*,#1919,.F.);
#2666=ORIENTED_EDGE('',*,*,#1922,.T.);
#2667=ORIENTED_EDGE('',*,*,#1923,.T.);
#2668=ORIENTED_EDGE('',*,*,#1924,.F.);
#2669=ORIENTED_EDGE('',*,*,#1920,.F.);
#2670=ORIENTED_EDGE('',*,*,#1925,.T.);
#2671=ORIENTED_EDGE('',*,*,#1926,.T.);
#2672=ORIENTED_EDGE('',*,*,#1927,.F.);
#2673=ORIENTED_EDGE('',*,*,#1915,.F.);
#2674=ORIENTED_EDGE('',*,*,#1928,.T.);
#2675=ORIENTED_EDGE('',*,*,#1929,.T.);
#2676=ORIENTED_EDGE('',*,*,#1930,.F.);
#2677=ORIENTED_EDGE('',*,*,#1931,.T.);
#2678=ORIENTED_EDGE('',*,*,#1932,.F.);
#2679=ORIENTED_EDGE('',*,*,#1933,.T.);
#2680=ORIENTED_EDGE('',*,*,#1934,.T.);
#2681=ORIENTED_EDGE('',*,*,#1909,.F.);
#2682=ORIENTED_EDGE('',*,*,#1935,.T.);
#2683=ORIENTED_EDGE('',*,*,#1936,.T.);
#2684=ORIENTED_EDGE('',*,*,#1937,.F.);
#2685=ORIENTED_EDGE('',*,*,#1938,.T.);
#2686=ORIENTED_EDGE('',*,*,#1939,.F.);
#2687=ORIENTED_EDGE('',*,*,#1940,.T.);
#2688=ORIENTED_EDGE('',*,*,#1941,.T.);
#2689=ORIENTED_EDGE('',*,*,#1911,.F.);
#2690=ORIENTED_EDGE('',*,*,#1942,.T.);
#2691=ORIENTED_EDGE('',*,*,#1943,.T.);
#2692=ORIENTED_EDGE('',*,*,#1944,.F.);
#2693=ORIENTED_EDGE('',*,*,#1945,.T.);
#2694=ORIENTED_EDGE('',*,*,#1946,.F.);
#2695=ORIENTED_EDGE('',*,*,#1947,.T.);
#2696=ORIENTED_EDGE('',*,*,#1948,.T.);
#2697=ORIENTED_EDGE('',*,*,#1904,.T.);
#2698=ORIENTED_EDGE('',*,*,#1949,.T.);
#2699=ORIENTED_EDGE('',*,*,#1950,.T.);
#2700=ORIENTED_EDGE('',*,*,#1951,.T.);
#2701=ORIENTED_EDGE('',*,*,#1950,.F.);
#2702=ORIENTED_EDGE('',*,*,#1887,.T.);
#2703=ORIENTED_EDGE('',*,*,#1888,.T.);
#2704=ORIENTED_EDGE('',*,*,#1951,.F.);
#2705=ORIENTED_EDGE('',*,*,#1895,.T.);
#2706=ORIENTED_EDGE('',*,*,#1905,.F.);
#2707=ORIENTED_EDGE('',*,*,#1902,.F.);
#2708=ORIENTED_EDGE('',*,*,#1900,.T.);
#2709=ORIENTED_EDGE('',*,*,#1890,.T.);
#2710=ORIENTED_EDGE('',*,*,#1918,.T.);
#2711=ORIENTED_EDGE('',*,*,#1952,.T.);
#2712=ORIENTED_EDGE('',*,*,#1953,.T.);
#2713=ORIENTED_EDGE('',*,*,#1952,.F.);
#2714=ORIENTED_EDGE('',*,*,#1953,.F.);
#2715=ORIENTED_EDGE('',*,*,#1949,.F.);
#2716=ORIENTED_EDGE('',*,*,#1945,.F.);
#2717=ORIENTED_EDGE('',*,*,#1954,.T.);
#2718=ORIENTED_EDGE('',*,*,#1955,.T.);
#2719=ORIENTED_EDGE('',*,*,#1956,.F.);
#2720=ORIENTED_EDGE('',*,*,#1944,.T.);
#2721=ORIENTED_EDGE('',*,*,#1957,.T.);
#2722=ORIENTED_EDGE('',*,*,#1958,.T.);
#2723=ORIENTED_EDGE('',*,*,#1954,.F.);
#2724=ORIENTED_EDGE('',*,*,#1943,.F.);
#2725=ORIENTED_EDGE('',*,*,#1959,.T.);
#2726=ORIENTED_EDGE('',*,*,#1960,.T.);
#2727=ORIENTED_EDGE('',*,*,#1957,.F.);
#2728=ORIENTED_EDGE('',*,*,#1942,.F.);
#2729=ORIENTED_EDGE('',*,*,#1910,.T.);
#2730=ORIENTED_EDGE('',*,*,#1924,.T.);
#2731=ORIENTED_EDGE('',*,*,#1961,.T.);
#2732=ORIENTED_EDGE('',*,*,#1959,.F.);
#2733=ORIENTED_EDGE('',*,*,#1948,.F.);
#2734=ORIENTED_EDGE('',*,*,#1962,.T.);
#2735=ORIENTED_EDGE('',*,*,#1963,.T.);
#2736=ORIENTED_EDGE('',*,*,#1922,.F.);
#2737=ORIENTED_EDGE('',*,*,#1916,.F.);
#2738=ORIENTED_EDGE('',*,*,#1947,.F.);
#2739=ORIENTED_EDGE('',*,*,#1964,.T.);
#2740=ORIENTED_EDGE('',*,*,#1965,.T.);
#2741=ORIENTED_EDGE('',*,*,#1962,.F.);
#2742=ORIENTED_EDGE('',*,*,#1946,.T.);
#2743=ORIENTED_EDGE('',*,*,#1956,.T.);
#2744=ORIENTED_EDGE('',*,*,#1966,.T.);
#2745=ORIENTED_EDGE('',*,*,#1964,.F.);
#2746=ORIENTED_EDGE('',*,*,#1966,.F.);
#2747=ORIENTED_EDGE('',*,*,#1955,.F.);
#2748=ORIENTED_EDGE('',*,*,#1958,.F.);
#2749=ORIENTED_EDGE('',*,*,#1960,.F.);
#2750=ORIENTED_EDGE('',*,*,#1961,.F.);
#2751=ORIENTED_EDGE('',*,*,#1923,.F.);
#2752=ORIENTED_EDGE('',*,*,#1963,.F.);
#2753=ORIENTED_EDGE('',*,*,#1965,.F.);
#2754=ORIENTED_EDGE('',*,*,#1938,.F.);
#2755=ORIENTED_EDGE('',*,*,#1967,.T.);
#2756=ORIENTED_EDGE('',*,*,#1968,.T.);
#2757=ORIENTED_EDGE('',*,*,#1969,.F.);
#2758=ORIENTED_EDGE('',*,*,#1937,.T.);
#2759=ORIENTED_EDGE('',*,*,#1970,.T.);
#2760=ORIENTED_EDGE('',*,*,#1971,.T.);
#2761=ORIENTED_EDGE('',*,*,#1967,.F.);
#2762=ORIENTED_EDGE('',*,*,#1936,.F.);
#2763=ORIENTED_EDGE('',*,*,#1972,.T.);
#2764=ORIENTED_EDGE('',*,*,#1973,.T.);
#2765=ORIENTED_EDGE('',*,*,#1970,.F.);
#2766=ORIENTED_EDGE('',*,*,#1935,.F.);
#2767=ORIENTED_EDGE('',*,*,#1908,.T.);
#2768=ORIENTED_EDGE('',*,*,#1927,.T.);
#2769=ORIENTED_EDGE('',*,*,#1974,.T.);
#2770=ORIENTED_EDGE('',*,*,#1972,.F.);
#2771=ORIENTED_EDGE('',*,*,#1941,.F.);
#2772=ORIENTED_EDGE('',*,*,#1975,.T.);
#2773=ORIENTED_EDGE('',*,*,#1976,.T.);
#2774=ORIENTED_EDGE('',*,*,#1925,.F.);
#2775=ORIENTED_EDGE('',*,*,#1912,.F.);
#2776=ORIENTED_EDGE('',*,*,#1940,.F.);
#2777=ORIENTED_EDGE('',*,*,#1977,.T.);
#2778=ORIENTED_EDGE('',*,*,#1978,.T.);
#2779=ORIENTED_EDGE('',*,*,#1975,.F.);
#2780=ORIENTED_EDGE('',*,*,#1939,.T.);
#2781=ORIENTED_EDGE('',*,*,#1969,.T.);
#2782=ORIENTED_EDGE('',*,*,#1979,.T.);
#2783=ORIENTED_EDGE('',*,*,#1977,.F.);
#2784=ORIENTED_EDGE('',*,*,#1979,.F.);
#2785=ORIENTED_EDGE('',*,*,#1968,.F.);
#2786=ORIENTED_EDGE('',*,*,#1971,.F.);
#2787=ORIENTED_EDGE('',*,*,#1973,.F.);
#2788=ORIENTED_EDGE('',*,*,#1974,.F.);
#2789=ORIENTED_EDGE('',*,*,#1926,.F.);
#2790=ORIENTED_EDGE('',*,*,#1976,.F.);
#2791=ORIENTED_EDGE('',*,*,#1978,.F.);
#2792=ORIENTED_EDGE('',*,*,#1931,.F.);
#2793=ORIENTED_EDGE('',*,*,#1980,.T.);
#2794=ORIENTED_EDGE('',*,*,#1981,.T.);
#2795=ORIENTED_EDGE('',*,*,#1982,.F.);
#2796=ORIENTED_EDGE('',*,*,#1930,.T.);
#2797=ORIENTED_EDGE('',*,*,#1983,.T.);
#2798=ORIENTED_EDGE('',*,*,#1984,.T.);
#2799=ORIENTED_EDGE('',*,*,#1980,.F.);
#2800=ORIENTED_EDGE('',*,*,#1929,.F.);
#2801=ORIENTED_EDGE('',*,*,#1985,.T.);
#2802=ORIENTED_EDGE('',*,*,#1986,.T.);
#2803=ORIENTED_EDGE('',*,*,#1983,.F.);
#2804=ORIENTED_EDGE('',*,*,#1928,.F.);
#2805=ORIENTED_EDGE('',*,*,#1914,.T.);
#2806=ORIENTED_EDGE('',*,*,#1987,.T.);
#2807=ORIENTED_EDGE('',*,*,#1988,.T.);
#2808=ORIENTED_EDGE('',*,*,#1985,.F.);
#2809=ORIENTED_EDGE('',*,*,#1921,.F.);
#2810=ORIENTED_EDGE('',*,*,#1989,.T.);
#2811=ORIENTED_EDGE('',*,*,#1990,.T.);
#2812=ORIENTED_EDGE('',*,*,#1987,.F.);
#2813=ORIENTED_EDGE('',*,*,#1934,.F.);
#2814=ORIENTED_EDGE('',*,*,#1991,.T.);
#2815=ORIENTED_EDGE('',*,*,#1992,.T.);
#2816=ORIENTED_EDGE('',*,*,#1989,.F.);
#2817=ORIENTED_EDGE('',*,*,#1906,.F.);
#2818=ORIENTED_EDGE('',*,*,#1933,.F.);
#2819=ORIENTED_EDGE('',*,*,#1993,.T.);
#2820=ORIENTED_EDGE('',*,*,#1994,.T.);
#2821=ORIENTED_EDGE('',*,*,#1991,.F.);
#2822=ORIENTED_EDGE('',*,*,#1932,.T.);
#2823=ORIENTED_EDGE('',*,*,#1982,.T.);
#2824=ORIENTED_EDGE('',*,*,#1995,.T.);
#2825=ORIENTED_EDGE('',*,*,#1993,.F.);
#2826=ORIENTED_EDGE('',*,*,#1995,.F.);
#2827=ORIENTED_EDGE('',*,*,#1981,.F.);
#2828=ORIENTED_EDGE('',*,*,#1984,.F.);
#2829=ORIENTED_EDGE('',*,*,#1986,.F.);
#2830=ORIENTED_EDGE('',*,*,#1988,.F.);
#2831=ORIENTED_EDGE('',*,*,#1990,.F.);
#2832=ORIENTED_EDGE('',*,*,#1992,.F.);
#2833=ORIENTED_EDGE('',*,*,#1994,.F.);
#2834=ORIENTED_EDGE('',*,*,#1996,.F.);
#2835=ORIENTED_EDGE('',*,*,#1997,.T.);
#2836=ORIENTED_EDGE('',*,*,#1998,.T.);
#2837=ORIENTED_EDGE('',*,*,#1999,.F.);
#2838=ORIENTED_EDGE('',*,*,#2000,.F.);
#2839=ORIENTED_EDGE('',*,*,#2001,.T.);
#2840=ORIENTED_EDGE('',*,*,#2002,.T.);
#2841=ORIENTED_EDGE('',*,*,#1997,.F.);
#2842=ORIENTED_EDGE('',*,*,#2003,.F.);
#2843=ORIENTED_EDGE('',*,*,#2004,.T.);
#2844=ORIENTED_EDGE('',*,*,#2005,.T.);
#2845=ORIENTED_EDGE('',*,*,#2001,.F.);
#2846=ORIENTED_EDGE('',*,*,#2006,.F.);
#2847=ORIENTED_EDGE('',*,*,#2007,.T.);
#2848=ORIENTED_EDGE('',*,*,#2008,.T.);
#2849=ORIENTED_EDGE('',*,*,#2004,.F.);
#2850=ORIENTED_EDGE('',*,*,#2009,.F.);
#2851=ORIENTED_EDGE('',*,*,#2010,.T.);
#2852=ORIENTED_EDGE('',*,*,#2011,.T.);
#2853=ORIENTED_EDGE('',*,*,#2007,.F.);
#2854=ORIENTED_EDGE('',*,*,#2012,.F.);
#2855=ORIENTED_EDGE('',*,*,#1999,.T.);
#2856=ORIENTED_EDGE('',*,*,#2013,.T.);
#2857=ORIENTED_EDGE('',*,*,#2010,.F.);
#2858=ORIENTED_EDGE('',*,*,#2013,.F.);
#2859=ORIENTED_EDGE('',*,*,#1998,.F.);
#2860=ORIENTED_EDGE('',*,*,#2002,.F.);
#2861=ORIENTED_EDGE('',*,*,#2005,.F.);
#2862=ORIENTED_EDGE('',*,*,#2008,.F.);
#2863=ORIENTED_EDGE('',*,*,#2011,.F.);
#2864=ORIENTED_EDGE('',*,*,#2014,.F.);
#2865=ORIENTED_EDGE('',*,*,#2015,.T.);
#2866=ORIENTED_EDGE('',*,*,#2016,.T.);
#2867=ORIENTED_EDGE('',*,*,#2015,.F.);
#2868=ORIENTED_EDGE('',*,*,#2014,.T.);
#2869=ORIENTED_EDGE('',*,*,#1996,.T.);
#2870=ORIENTED_EDGE('',*,*,#2012,.T.);
#2871=ORIENTED_EDGE('',*,*,#2009,.T.);
#2872=ORIENTED_EDGE('',*,*,#2006,.T.);
#2873=ORIENTED_EDGE('',*,*,#2003,.T.);
#2874=ORIENTED_EDGE('',*,*,#2000,.T.);
#2875=ORIENTED_EDGE('',*,*,#2016,.F.);
#2876=ORIENTED_EDGE('',*,*,#2017,.T.);
#2877=ORIENTED_EDGE('',*,*,#2018,.T.);
#2878=ORIENTED_EDGE('',*,*,#2019,.F.);
#2879=ORIENTED_EDGE('',*,*,#2020,.F.);
#2880=ORIENTED_EDGE('',*,*,#2021,.T.);
#2881=ORIENTED_EDGE('',*,*,#2020,.T.);
#2882=ORIENTED_EDGE('',*,*,#2022,.F.);
#2883=ORIENTED_EDGE('',*,*,#2023,.F.);
#2884=ORIENTED_EDGE('',*,*,#2024,.T.);
#2885=ORIENTED_EDGE('',*,*,#2023,.T.);
#2886=ORIENTED_EDGE('',*,*,#2025,.F.);
#2887=ORIENTED_EDGE('',*,*,#2026,.F.);
#2888=ORIENTED_EDGE('',*,*,#2027,.T.);
#2889=ORIENTED_EDGE('',*,*,#2026,.T.);
#2890=ORIENTED_EDGE('',*,*,#2028,.F.);
#2891=ORIENTED_EDGE('',*,*,#2029,.F.);
#2892=ORIENTED_EDGE('',*,*,#2030,.T.);
#2893=ORIENTED_EDGE('',*,*,#2029,.T.);
#2894=ORIENTED_EDGE('',*,*,#2031,.F.);
#2895=ORIENTED_EDGE('',*,*,#2032,.F.);
#2896=ORIENTED_EDGE('',*,*,#2033,.T.);
#2897=ORIENTED_EDGE('',*,*,#2032,.T.);
#2898=ORIENTED_EDGE('',*,*,#2034,.F.);
#2899=ORIENTED_EDGE('',*,*,#2018,.F.);
#2900=ORIENTED_EDGE('',*,*,#2034,.T.);
#2901=ORIENTED_EDGE('',*,*,#2031,.T.);
#2902=ORIENTED_EDGE('',*,*,#2028,.T.);
#2903=ORIENTED_EDGE('',*,*,#2025,.T.);
#2904=ORIENTED_EDGE('',*,*,#2022,.T.);
#2905=ORIENTED_EDGE('',*,*,#2019,.T.);
#2906=ORIENTED_EDGE('',*,*,#2035,.F.);
#2907=ORIENTED_EDGE('',*,*,#2036,.T.);
#2908=ORIENTED_EDGE('',*,*,#2037,.T.);
#2909=ORIENTED_EDGE('',*,*,#2036,.F.);
#2910=ORIENTED_EDGE('',*,*,#2037,.F.);
#2911=ORIENTED_EDGE('',*,*,#2017,.F.);
#2912=ORIENTED_EDGE('',*,*,#2021,.F.);
#2913=ORIENTED_EDGE('',*,*,#2024,.F.);
#2914=ORIENTED_EDGE('',*,*,#2027,.F.);
#2915=ORIENTED_EDGE('',*,*,#2030,.F.);
#2916=ORIENTED_EDGE('',*,*,#2033,.F.);
#2917=ORIENTED_EDGE('',*,*,#2035,.T.);
#2918=ORIENTED_EDGE('',*,*,#2038,.F.);
#2919=ORIENTED_EDGE('',*,*,#2039,.F.);
#2920=ORIENTED_EDGE('',*,*,#2040,.F.);
#2921=ORIENTED_EDGE('',*,*,#2041,.T.);
#2922=ORIENTED_EDGE('',*,*,#2042,.F.);
#2923=ORIENTED_EDGE('',*,*,#2041,.F.);
#2924=ORIENTED_EDGE('',*,*,#2043,.F.);
#2925=ORIENTED_EDGE('',*,*,#2044,.T.);
#2926=ORIENTED_EDGE('',*,*,#2043,.T.);
#2927=ORIENTED_EDGE('',*,*,#2040,.T.);
#2928=ORIENTED_EDGE('',*,*,#2045,.T.);
#2929=ORIENTED_EDGE('',*,*,#2046,.T.);
#2930=ORIENTED_EDGE('',*,*,#2047,.F.);
#2931=ORIENTED_EDGE('',*,*,#2044,.F.);
#2932=ORIENTED_EDGE('',*,*,#2046,.F.);
#2933=ORIENTED_EDGE('',*,*,#2048,.T.);
#2934=ORIENTED_EDGE('',*,*,#2049,.F.);
#2935=ORIENTED_EDGE('',*,*,#2048,.F.);
#2936=ORIENTED_EDGE('',*,*,#2045,.F.);
#2937=ORIENTED_EDGE('',*,*,#2039,.T.);
#2938=ORIENTED_EDGE('',*,*,#2050,.T.);
#2939=ORIENTED_EDGE('',*,*,#2051,.F.);
#2940=ORIENTED_EDGE('',*,*,#2052,.T.);
#2941=ORIENTED_EDGE('',*,*,#2050,.F.);
#2942=ORIENTED_EDGE('',*,*,#2052,.F.);
#2943=ORIENTED_EDGE('',*,*,#2047,.T.);
#2944=ORIENTED_EDGE('',*,*,#2049,.T.);
#2945=ORIENTED_EDGE('',*,*,#2038,.T.);
#2946=ORIENTED_EDGE('',*,*,#2042,.T.);
#2947=ORIENTED_EDGE('',*,*,#2051,.T.);
#2948=ORIENTED_EDGE('',*,*,#2053,.T.);
#2949=ORIENTED_EDGE('',*,*,#2054,.F.);
#2950=ORIENTED_EDGE('',*,*,#2055,.T.);
#2951=ORIENTED_EDGE('',*,*,#2056,.T.);
#2952=ORIENTED_EDGE('',*,*,#2057,.T.);
#2953=ORIENTED_EDGE('',*,*,#2058,.F.);
#2954=ORIENTED_EDGE('',*,*,#2059,.T.);
#2955=ORIENTED_EDGE('',*,*,#2054,.T.);
#2956=ORIENTED_EDGE('',*,*,#2059,.F.);
#2957=ORIENTED_EDGE('',*,*,#2060,.F.);
#2958=ORIENTED_EDGE('',*,*,#2061,.F.);
#2959=ORIENTED_EDGE('',*,*,#2055,.F.);
#2960=ORIENTED_EDGE('',*,*,#2062,.T.);
#2961=ORIENTED_EDGE('',*,*,#2063,.F.);
#2962=ORIENTED_EDGE('',*,*,#2060,.T.);
#2963=ORIENTED_EDGE('',*,*,#2058,.T.);
#2964=ORIENTED_EDGE('',*,*,#2064,.T.);
#2965=ORIENTED_EDGE('',*,*,#2056,.F.);
#2966=ORIENTED_EDGE('',*,*,#2061,.T.);
#2967=ORIENTED_EDGE('',*,*,#2063,.T.);
#2968=ORIENTED_EDGE('',*,*,#2065,.F.);
#2969=ORIENTED_EDGE('',*,*,#2065,.T.);
#2970=ORIENTED_EDGE('',*,*,#2066,.T.);
#2971=ORIENTED_EDGE('',*,*,#2067,.T.);
#2972=ORIENTED_EDGE('',*,*,#2066,.F.);
#2973=ORIENTED_EDGE('',*,*,#2062,.F.);
#2974=ORIENTED_EDGE('',*,*,#2057,.F.);
#2975=ORIENTED_EDGE('',*,*,#2053,.F.);
#2976=ORIENTED_EDGE('',*,*,#2064,.F.);
#2977=ORIENTED_EDGE('',*,*,#2067,.F.);
#2978=ORIENTED_EDGE('',*,*,#2068,.T.);
#2979=ORIENTED_EDGE('',*,*,#2069,.T.);
#2980=ORIENTED_EDGE('',*,*,#2070,.T.);
#2981=ORIENTED_EDGE('',*,*,#2071,.T.);
#2982=ORIENTED_EDGE('',*,*,#2071,.F.);
#2983=ORIENTED_EDGE('',*,*,#2072,.T.);
#2984=ORIENTED_EDGE('',*,*,#2073,.T.);
#2985=ORIENTED_EDGE('',*,*,#2074,.F.);
#2986=ORIENTED_EDGE('',*,*,#2068,.F.);
#2987=ORIENTED_EDGE('',*,*,#2074,.T.);
#2988=ORIENTED_EDGE('',*,*,#2075,.T.);
#2989=ORIENTED_EDGE('',*,*,#2076,.F.);
#2990=ORIENTED_EDGE('',*,*,#2070,.F.);
#2991=ORIENTED_EDGE('',*,*,#2077,.T.);
#2992=ORIENTED_EDGE('',*,*,#2078,.T.);
#2993=ORIENTED_EDGE('',*,*,#2072,.F.);
#2994=ORIENTED_EDGE('',*,*,#2069,.F.);
#2995=ORIENTED_EDGE('',*,*,#2076,.T.);
#2996=ORIENTED_EDGE('',*,*,#2079,.T.);
#2997=ORIENTED_EDGE('',*,*,#2077,.F.);
#2998=ORIENTED_EDGE('',*,*,#2075,.F.);
#2999=ORIENTED_EDGE('',*,*,#2073,.F.);
#3000=ORIENTED_EDGE('',*,*,#2078,.F.);
#3001=ORIENTED_EDGE('',*,*,#2079,.F.);
#3002=ORIENTED_EDGE('',*,*,#2080,.F.);
#3003=ORIENTED_EDGE('',*,*,#2081,.F.);
#3004=ORIENTED_EDGE('',*,*,#2082,.F.);
#3005=ORIENTED_EDGE('',*,*,#2083,.F.);
#3006=ORIENTED_EDGE('',*,*,#2081,.T.);
#3007=ORIENTED_EDGE('',*,*,#2084,.T.);
#3008=ORIENTED_EDGE('',*,*,#2085,.F.);
#3009=ORIENTED_EDGE('',*,*,#2086,.F.);
#3010=ORIENTED_EDGE('',*,*,#2080,.T.);
#3011=ORIENTED_EDGE('',*,*,#2087,.T.);
#3012=ORIENTED_EDGE('',*,*,#2088,.F.);
#3013=ORIENTED_EDGE('',*,*,#2084,.F.);
#3014=ORIENTED_EDGE('',*,*,#2082,.T.);
#3015=ORIENTED_EDGE('',*,*,#2086,.T.);
#3016=ORIENTED_EDGE('',*,*,#2089,.F.);
#3017=ORIENTED_EDGE('',*,*,#2090,.F.);
#3018=ORIENTED_EDGE('',*,*,#2083,.T.);
#3019=ORIENTED_EDGE('',*,*,#2090,.T.);
#3020=ORIENTED_EDGE('',*,*,#2091,.F.);
#3021=ORIENTED_EDGE('',*,*,#2087,.F.);
#3022=ORIENTED_EDGE('',*,*,#2088,.T.);
#3023=ORIENTED_EDGE('',*,*,#2091,.T.);
#3024=ORIENTED_EDGE('',*,*,#2089,.T.);
#3025=ORIENTED_EDGE('',*,*,#2085,.T.);
#3026=CYLINDRICAL_SURFACE('',#3399,1.);
#3027=CYLINDRICAL_SURFACE('',#3403,1.);
#3028=CYLINDRICAL_SURFACE('',#3407,1.);
#3029=CYLINDRICAL_SURFACE('',#3411,1.);
#3030=CYLINDRICAL_SURFACE('',#3415,1.);
#3031=CYLINDRICAL_SURFACE('',#3419,1.);
#3032=CYLINDRICAL_SURFACE('',#3423,1.);
#3033=CYLINDRICAL_SURFACE('',#3427,1.);
#3034=CYLINDRICAL_SURFACE('',#3431,1.);
#3035=CYLINDRICAL_SURFACE('',#3435,1.);
#3036=CYLINDRICAL_SURFACE('',#3439,11.9999999999996);
#3037=CYLINDRICAL_SURFACE('',#3442,11.9999999999996);
#3038=CYLINDRICAL_SURFACE('',#3445,11.9999999999996);
#3039=CYLINDRICAL_SURFACE('',#3448,11.9999999999996);
#3040=CYLINDRICAL_SURFACE('',#3451,11.9999999999996);
#3041=CYLINDRICAL_SURFACE('',#3465,5.529);
#3042=CYLINDRICAL_SURFACE('',#3467,5.529);
#3043=CYLINDRICAL_SURFACE('',#3469,5.529);
#3044=CYLINDRICAL_SURFACE('',#3471,5.529);
#3045=CYLINDRICAL_SURFACE('',#3473,5.529);
#3046=CYLINDRICAL_SURFACE('',#3475,1.);
#3047=CYLINDRICAL_SURFACE('',#3478,1.);
#3048=CYLINDRICAL_SURFACE('',#3481,11.9999999999996);
#3049=CYLINDRICAL_SURFACE('',#3486,5.);
#3050=CYLINDRICAL_SURFACE('',#3487,5.529);
#3051=CYLINDRICAL_SURFACE('',#3489,1.);
#3052=CYLINDRICAL_SURFACE('',#3495,1.);
#3053=CYLINDRICAL_SURFACE('',#3498,5.);
#3054=CYLINDRICAL_SURFACE('',#3502,12.);
#3055=CYLINDRICAL_SURFACE('',#3505,12.);
#3056=CYLINDRICAL_SURFACE('',#3508,12.);
#3057=CYLINDRICAL_SURFACE('',#3516,12.);
#3058=CYLINDRICAL_SURFACE('',#3518,12.);
#3059=CYLINDRICAL_SURFACE('',#3530,7.);
#3060=CYLINDRICAL_SURFACE('',#3534,13.5);
#3061=CYLINDRICAL_SURFACE('',#3537,5.529);
#3062=CYLINDRICAL_SURFACE('',#3539,1.);
#3063=CYLINDRICAL_SURFACE('',#3543,1.);
#3064=CYLINDRICAL_SURFACE('',#3546,5.529);
#3065=CYLINDRICAL_SURFACE('',#3548,1.);
#3066=CYLINDRICAL_SURFACE('',#3552,1.);
#3067=CYLINDRICAL_SURFACE('',#3555,5.529);
#3068=CYLINDRICAL_SURFACE('',#3557,1.);
#3069=CYLINDRICAL_SURFACE('',#3560,12.);
#3070=CYLINDRICAL_SURFACE('',#3563,1.);
#3071=CYLINDRICAL_SURFACE('',#3567,1.);
#3072=CYLINDRICAL_SURFACE('',#3574,1.);
#3073=CYLINDRICAL_SURFACE('',#3576,5.);
#3074=CYLINDRICAL_SURFACE('',#3580,12.);
#3075=CYLINDRICAL_SURFACE('',#3583,12.);
#3076=CYLINDRICAL_SURFACE('',#3586,12.);
#3077=CYLINDRICAL_SURFACE('',#3594,12.);
#3078=CYLINDRICAL_SURFACE('',#3596,12.);
#3079=CYLINDRICAL_SURFACE('',#3608,7.);
#3080=CYLINDRICAL_SURFACE('',#3612,13.5);
#3081=CYLINDRICAL_SURFACE('',#3615,5.529);
#3082=CYLINDRICAL_SURFACE('',#3617,1.);
#3083=CYLINDRICAL_SURFACE('',#3621,1.);
#3084=CYLINDRICAL_SURFACE('',#3624,5.529);
#3085=CYLINDRICAL_SURFACE('',#3626,1.);
#3086=CYLINDRICAL_SURFACE('',#3630,1.);
#3087=CYLINDRICAL_SURFACE('',#3633,5.529);
#3088=CYLINDRICAL_SURFACE('',#3635,1.);
#3089=CYLINDRICAL_SURFACE('',#3638,12.);
#3090=CYLINDRICAL_SURFACE('',#3641,1.);
#3091=CYLINDRICAL_SURFACE('',#3652,1.);
#3092=CYLINDRICAL_SURFACE('',#3665,1.);
#3093=CYLINDRICAL_SURFACE('',#3672,1.);
#3094=CYLINDRICAL_SURFACE('',#3677,1.);
#3095=CYLINDRICAL_SURFACE('',#3680,5.);
#3096=CYLINDRICAL_SURFACE('',#3685,1.);
#3097=CYLINDRICAL_SURFACE('',#3690,1.);
#3098=CYLINDRICAL_SURFACE('',#3693,5.);
#3099=CYLINDRICAL_SURFACE('',#3701,1.);
#3100=CYLINDRICAL_SURFACE('',#3703,1.);
#3101=CYLINDRICAL_SURFACE('',#3712,1.);
#3102=CYLINDRICAL_SURFACE('',#3714,1.);
#3103=ADVANCED_FACE('',(#265),#3026,.F.);
#3104=ADVANCED_FACE('',(#266),#181,.T.);
#3105=ADVANCED_FACE('',(#267),#3027,.F.);
#3106=ADVANCED_FACE('',(#268),#182,.T.);
#3107=ADVANCED_FACE('',(#269),#3028,.F.);
#3108=ADVANCED_FACE('',(#270),#183,.T.);
#3109=ADVANCED_FACE('',(#271),#3029,.F.);
#3110=ADVANCED_FACE('',(#272),#184,.T.);
#3111=ADVANCED_FACE('',(#273),#3030,.F.);
#3112=ADVANCED_FACE('',(#274),#185,.T.);
#3113=ADVANCED_FACE('',(#275),#3031,.F.);
#3114=ADVANCED_FACE('',(#276),#186,.T.);
#3115=ADVANCED_FACE('',(#277),#3032,.F.);
#3116=ADVANCED_FACE('',(#278),#187,.T.);
#3117=ADVANCED_FACE('',(#279),#3033,.F.);
#3118=ADVANCED_FACE('',(#280),#188,.T.);
#3119=ADVANCED_FACE('',(#281),#3034,.F.);
#3120=ADVANCED_FACE('',(#282),#189,.T.);
#3121=ADVANCED_FACE('',(#283),#3035,.F.);
#3122=ADVANCED_FACE('',(#284),#190,.T.);
#3123=ADVANCED_FACE('',(#285),#157,.T.);
#3124=ADVANCED_FACE('',(#286),#3036,.T.);
#3125=ADVANCED_FACE('',(#287),#158,.T.);
#3126=ADVANCED_FACE('',(#288),#159,.T.);
#3127=ADVANCED_FACE('',(#289),#3037,.T.);
#3128=ADVANCED_FACE('',(#290),#160,.T.);
#3129=ADVANCED_FACE('',(#291),#161,.T.);
#3130=ADVANCED_FACE('',(#292),#3038,.T.);
#3131=ADVANCED_FACE('',(#293),#162,.T.);
#3132=ADVANCED_FACE('',(#294),#163,.T.);
#3133=ADVANCED_FACE('',(#295),#3039,.T.);
#3134=ADVANCED_FACE('',(#296),#164,.T.);
#3135=ADVANCED_FACE('',(#297),#165,.T.);
#3136=ADVANCED_FACE('',(#298),#3040,.T.);
#3137=ADVANCED_FACE('',(#299),#166,.T.);
#3138=ADVANCED_FACE('',(#300,#83),#191,.F.);
#3139=ADVANCED_FACE('',(#301),#3041,.T.);
#3140=ADVANCED_FACE('',(#302),#3042,.T.);
#3141=ADVANCED_FACE('',(#303),#3043,.T.);
#3142=ADVANCED_FACE('',(#304),#3044,.T.);
#3143=ADVANCED_FACE('',(#305),#3045,.T.);
#3144=ADVANCED_FACE('',(#306),#3046,.F.);
#3145=ADVANCED_FACE('',(#307),#192,.T.);
#3146=ADVANCED_FACE('',(#308),#3047,.F.);
#3147=ADVANCED_FACE('',(#309),#193,.T.);
#3148=ADVANCED_FACE('',(#310),#167,.T.);
#3149=ADVANCED_FACE('',(#311),#3048,.T.);
#3150=ADVANCED_FACE('',(#312),#168,.T.);
#3151=ADVANCED_FACE('',(#313,#84),#194,.T.);
#3152=ADVANCED_FACE('',(#314),#3049,.F.);
#3153=ADVANCED_FACE('',(#315),#3050,.T.);
#3154=ADVANCED_FACE('',(#316),#3051,.F.);
#3155=ADVANCED_FACE('',(#317),#195,.T.);
#3156=ADVANCED_FACE('',(#318),#196,.T.);
#3157=ADVANCED_FACE('',(#319),#3052,.F.);
#3158=ADVANCED_FACE('',(#320),#197,.F.);
#3159=ADVANCED_FACE('',(#321),#198,.F.);
#3160=ADVANCED_FACE('',(#322),#3053,.F.);
#3161=ADVANCED_FACE('',(#323),#3054,.F.);
#3162=ADVANCED_FACE('',(#324),#3055,.F.);
#3163=ADVANCED_FACE('',(#325),#3056,.F.);
#3164=ADVANCED_FACE('',(#326,#85),#199,.F.);
#3165=ADVANCED_FACE('',(#327),#3057,.T.);
#3166=ADVANCED_FACE('',(#328),#3058,.T.);
#3167=ADVANCED_FACE('',(#329,#86),#200,.F.);
#3168=ADVANCED_FACE('',(#330,#87),#3059,.T.);
#3169=ADVANCED_FACE('',(#331,#88),#201,.T.);
#3170=ADVANCED_FACE('',(#332),#3060,.T.);
#3171=ADVANCED_FACE('',(#333,#89),#202,.T.);
#3172=ADVANCED_FACE('',(#334),#3061,.F.);
#3173=ADVANCED_FACE('',(#335),#3062,.T.);
#3174=ADVANCED_FACE('',(#336),#203,.T.);
#3175=ADVANCED_FACE('',(#337),#169,.T.);
#3176=ADVANCED_FACE('',(#338),#170,.T.);
#3177=ADVANCED_FACE('',(#339),#204,.T.);
#3178=ADVANCED_FACE('',(#340),#3063,.T.);
#3179=ADVANCED_FACE('',(#341),#205,.F.);
#3180=ADVANCED_FACE('',(#342),#3064,.F.);
#3181=ADVANCED_FACE('',(#343),#3065,.T.);
#3182=ADVANCED_FACE('',(#344),#206,.T.);
#3183=ADVANCED_FACE('',(#345),#171,.T.);
#3184=ADVANCED_FACE('',(#346),#172,.T.);
#3185=ADVANCED_FACE('',(#347),#207,.T.);
#3186=ADVANCED_FACE('',(#348),#3066,.T.);
#3187=ADVANCED_FACE('',(#349),#208,.F.);
#3188=ADVANCED_FACE('',(#350),#3067,.F.);
#3189=ADVANCED_FACE('',(#351),#3068,.T.);
#3190=ADVANCED_FACE('',(#352),#209,.T.);
#3191=ADVANCED_FACE('',(#353),#173,.T.);
#3192=ADVANCED_FACE('',(#354),#3069,.T.);
#3193=ADVANCED_FACE('',(#355),#174,.T.);
#3194=ADVANCED_FACE('',(#356),#210,.T.);
#3195=ADVANCED_FACE('',(#357),#3070,.T.);
#3196=ADVANCED_FACE('',(#358),#211,.F.);
#3197=ADVANCED_FACE('',(#359),#3071,.F.);
#3198=ADVANCED_FACE('',(#360),#212,.F.);
#3199=ADVANCED_FACE('',(#361),#213,.F.);
#3200=ADVANCED_FACE('',(#362),#214,.T.);
#3201=ADVANCED_FACE('',(#363),#3072,.F.);
#3202=ADVANCED_FACE('',(#364),#215,.T.);
#3203=ADVANCED_FACE('',(#365),#3073,.F.);
#3204=ADVANCED_FACE('',(#366),#3074,.F.);
#3205=ADVANCED_FACE('',(#367),#3075,.F.);
#3206=ADVANCED_FACE('',(#368),#3076,.F.);
#3207=ADVANCED_FACE('',(#369,#90),#216,.T.);
#3208=ADVANCED_FACE('',(#370),#3077,.T.);
#3209=ADVANCED_FACE('',(#371),#3078,.T.);
#3210=ADVANCED_FACE('',(#372,#91),#217,.T.);
#3211=ADVANCED_FACE('',(#373,#92),#3079,.T.);
#3212=ADVANCED_FACE('',(#374,#93),#218,.F.);
#3213=ADVANCED_FACE('',(#375),#3080,.T.);
#3214=ADVANCED_FACE('',(#376,#94),#219,.F.);
#3215=ADVANCED_FACE('',(#377),#3081,.F.);
#3216=ADVANCED_FACE('',(#378),#3082,.T.);
#3217=ADVANCED_FACE('',(#379),#220,.F.);
#3218=ADVANCED_FACE('',(#380),#175,.F.);
#3219=ADVANCED_FACE('',(#381),#176,.F.);
#3220=ADVANCED_FACE('',(#382),#221,.F.);
#3221=ADVANCED_FACE('',(#383),#3083,.T.);
#3222=ADVANCED_FACE('',(#384),#222,.T.);
#3223=ADVANCED_FACE('',(#385),#3084,.F.);
#3224=ADVANCED_FACE('',(#386),#3085,.T.);
#3225=ADVANCED_FACE('',(#387),#223,.F.);
#3226=ADVANCED_FACE('',(#388),#177,.F.);
#3227=ADVANCED_FACE('',(#389),#178,.F.);
#3228=ADVANCED_FACE('',(#390),#224,.F.);
#3229=ADVANCED_FACE('',(#391),#3086,.T.);
#3230=ADVANCED_FACE('',(#392),#225,.T.);
#3231=ADVANCED_FACE('',(#393),#3087,.F.);
#3232=ADVANCED_FACE('',(#394),#3088,.T.);
#3233=ADVANCED_FACE('',(#395),#226,.F.);
#3234=ADVANCED_FACE('',(#396),#179,.F.);
#3235=ADVANCED_FACE('',(#397),#3089,.T.);
#3236=ADVANCED_FACE('',(#398),#180,.F.);
#3237=ADVANCED_FACE('',(#399),#227,.F.);
#3238=ADVANCED_FACE('',(#400),#3090,.T.);
#3239=ADVANCED_FACE('',(#401),#228,.T.);
#3240=ADVANCED_FACE('',(#402),#229,.F.);
#3241=ADVANCED_FACE('',(#403),#230,.F.);
#3242=ADVANCED_FACE('',(#404),#231,.F.);
#3243=ADVANCED_FACE('',(#405),#232,.F.);
#3244=ADVANCED_FACE('',(#406),#233,.F.);
#3245=ADVANCED_FACE('',(#407),#234,.F.);
#3246=ADVANCED_FACE('',(#408),#235,.F.);
#3247=ADVANCED_FACE('',(#409),#3091,.T.);
#3248=ADVANCED_FACE('',(#410,#95),#236,.T.);
#3249=ADVANCED_FACE('',(#411),#237,.F.);
#3250=ADVANCED_FACE('',(#412),#238,.T.);
#3251=ADVANCED_FACE('',(#413),#239,.T.);
#3252=ADVANCED_FACE('',(#414),#240,.T.);
#3253=ADVANCED_FACE('',(#415),#241,.T.);
#3254=ADVANCED_FACE('',(#416),#242,.T.);
#3255=ADVANCED_FACE('',(#417),#243,.T.);
#3256=ADVANCED_FACE('',(#418),#244,.T.);
#3257=ADVANCED_FACE('',(#419),#3092,.T.);
#3258=ADVANCED_FACE('',(#420,#96),#245,.F.);
#3259=ADVANCED_FACE('',(#421),#246,.T.);
#3260=ADVANCED_FACE('',(#422),#247,.F.);
#3261=ADVANCED_FACE('',(#423),#3093,.F.);
#3262=ADVANCED_FACE('',(#424),#248,.F.);
#3263=ADVANCED_FACE('',(#425),#249,.F.);
#3264=ADVANCED_FACE('',(#426),#3094,.F.);
#3265=ADVANCED_FACE('',(#427),#250,.F.);
#3266=ADVANCED_FACE('',(#428,#97),#3095,.T.);
#3267=ADVANCED_FACE('',(#429),#251,.T.);
#3268=ADVANCED_FACE('',(#430),#252,.T.);
#3269=ADVANCED_FACE('',(#431),#3096,.F.);
#3270=ADVANCED_FACE('',(#432),#253,.T.);
#3271=ADVANCED_FACE('',(#433),#254,.T.);
#3272=ADVANCED_FACE('',(#434),#3097,.F.);
#3273=ADVANCED_FACE('',(#435),#255,.T.);
#3274=ADVANCED_FACE('',(#436,#98),#3098,.T.);
#3275=ADVANCED_FACE('',(#437),#256,.F.);
#3276=ADVANCED_FACE('',(#438),#257,.F.);
#3277=ADVANCED_FACE('',(#439),#258,.F.);
#3278=ADVANCED_FACE('',(#440),#3099,.T.);
#3279=ADVANCED_FACE('',(#441),#3100,.T.);
#3280=ADVANCED_FACE('',(#442),#259,.F.);
#3281=ADVANCED_FACE('',(#443),#260,.T.);
#3282=ADVANCED_FACE('',(#444),#261,.T.);
#3283=ADVANCED_FACE('',(#445),#262,.T.);
#3284=ADVANCED_FACE('',(#446),#3101,.T.);
#3285=ADVANCED_FACE('',(#447),#3102,.T.);
#3286=ADVANCED_FACE('',(#448),#263,.T.);
#3287=ADVANCED_FACE('',(#449),#264,.F.);
#3288=CLOSED_SHELL('',(#3103,#3104,#3105,#3106,#3107,#3108,#3109,#3110,
#3111,#3112,#3113,#3114,#3115,#3116,#3117,#3118,#3119,#3120,#3121,#3122,
#3123,#3124,#3125,#3126,#3127,#3128,#3129,#3130,#3131,#3132,#3133,#3134,
#3135,#3136,#3137,#3138,#3139,#3140,#3141,#3142,#3143,#3144,#3145,#3146,
#3147,#3148,#3149,#3150,#3151,#3152,#3153));
#3289=CLOSED_SHELL('',(#3154,#3155,#3156,#3157,#3158,#3159,#3160,#3161,
#3162,#3163,#3164,#3165,#3166,#3167,#3168,#3169,#3170,#3171,#3172,#3173,
#3174,#3175,#3176,#3177,#3178,#3179,#3180,#3181,#3182,#3183,#3184,#3185,
#3186,#3187,#3188,#3189,#3190,#3191,#3192,#3193,#3194,#3195,#3196));
#3290=CLOSED_SHELL('',(#3197,#3198,#3199,#3200,#3201,#3202,#3203,#3204,
#3205,#3206,#3207,#3208,#3209,#3210,#3211,#3212,#3213,#3214,#3215,#3216,
#3217,#3218,#3219,#3220,#3221,#3222,#3223,#3224,#3225,#3226,#3227,#3228,
#3229,#3230,#3231,#3232,#3233,#3234,#3235,#3236,#3237,#3238,#3239));
#3291=CLOSED_SHELL('',(#3240,#3241,#3242,#3243,#3244,#3245,#3246,#3247,
#3248,#3249));
#3292=CLOSED_SHELL('',(#3250,#3251,#3252,#3253,#3254,#3255,#3256,#3257,
#3258,#3259));
#3293=CLOSED_SHELL('',(#3260,#3261,#3262,#3263,#3264,#3265,#3266,#3267));
#3294=CLOSED_SHELL('',(#3268,#3269,#3270,#3271,#3272,#3273,#3274,#3275));
#3295=CLOSED_SHELL('',(#3276,#3277,#3278,#3279,#3280,#3281));
#3296=CLOSED_SHELL('',(#3282,#3283,#3284,#3285,#3286,#3287));
#3297=DERIVED_UNIT_ELEMENT(#3315,1.);
#3298=DERIVED_UNIT_ELEMENT(#9824,-3.);
#3299=DERIVED_UNIT_ELEMENT(#3315,1.);
#3300=DERIVED_UNIT_ELEMENT(#9824,-3.);
#3301=DERIVED_UNIT_ELEMENT(#3315,1.);
#3302=DERIVED_UNIT_ELEMENT(#9824,-3.);
#3303=DERIVED_UNIT_ELEMENT(#3315,1.);
#3304=DERIVED_UNIT_ELEMENT(#9824,-3.);
#3305=DERIVED_UNIT_ELEMENT(#3315,1.);
#3306=DERIVED_UNIT_ELEMENT(#9824,-3.);
#3307=DERIVED_UNIT_ELEMENT(#3315,1.);
#3308=DERIVED_UNIT_ELEMENT(#9824,-3.);
#3309=DERIVED_UNIT_ELEMENT(#3315,1.);
#3310=DERIVED_UNIT_ELEMENT(#9824,-3.);
#3311=DERIVED_UNIT_ELEMENT(#3315,1.);
#3312=DERIVED_UNIT_ELEMENT(#9824,-3.);
#3313=DERIVED_UNIT_ELEMENT(#3315,1.);
#3314=DERIVED_UNIT_ELEMENT(#9824,-3.);
#3315=(
MASS_UNIT()
NAMED_UNIT(*)
SI_UNIT(.KILO.,.GRAM.)
);
#3316=DERIVED_UNIT((#3297,#3298));
#3317=DERIVED_UNIT((#3299,#3300));
#3318=DERIVED_UNIT((#3301,#3302));
#3319=DERIVED_UNIT((#3303,#3304));
#3320=DERIVED_UNIT((#3305,#3306));
#3321=DERIVED_UNIT((#3307,#3308));
#3322=DERIVED_UNIT((#3309,#3310));
#3323=DERIVED_UNIT((#3311,#3312));
#3324=DERIVED_UNIT((#3313,#3314));
#3325=MEASURE_REPRESENTATION_ITEM('density measure',
POSITIVE_RATIO_MEASURE(7850.),#3316);
#3326=MEASURE_REPRESENTATION_ITEM('density measure',
POSITIVE_RATIO_MEASURE(7850.),#3317);
#3327=MEASURE_REPRESENTATION_ITEM('density measure',
POSITIVE_RATIO_MEASURE(7850.),#3318);
#3328=MEASURE_REPRESENTATION_ITEM('density measure',
POSITIVE_RATIO_MEASURE(7850.),#3319);
#3329=MEASURE_REPRESENTATION_ITEM('density measure',
POSITIVE_RATIO_MEASURE(7850.),#3320);
#3330=MEASURE_REPRESENTATION_ITEM('density measure',
POSITIVE_RATIO_MEASURE(7850.),#3321);
#3331=MEASURE_REPRESENTATION_ITEM('density measure',
POSITIVE_RATIO_MEASURE(7850.),#3322);
#3332=MEASURE_REPRESENTATION_ITEM('density measure',
POSITIVE_RATIO_MEASURE(7850.),#3323);
#3333=MEASURE_REPRESENTATION_ITEM('density measure',
POSITIVE_RATIO_MEASURE(7850.),#3324);
#3334=PROPERTY_DEFINITION_REPRESENTATION(#3379,#3352);
#3335=PROPERTY_DEFINITION_REPRESENTATION(#3380,#3353);
#3336=PROPERTY_DEFINITION_REPRESENTATION(#3381,#3354);
#3337=PROPERTY_DEFINITION_REPRESENTATION(#3382,#3355);
#3338=PROPERTY_DEFINITION_REPRESENTATION(#3383,#3356);
#3339=PROPERTY_DEFINITION_REPRESENTATION(#3384,#3357);
#3340=PROPERTY_DEFINITION_REPRESENTATION(#3385,#3358);
#3341=PROPERTY_DEFINITION_REPRESENTATION(#3386,#3359);
#3342=PROPERTY_DEFINITION_REPRESENTATION(#3387,#3360);
#3343=PROPERTY_DEFINITION_REPRESENTATION(#3388,#3361);
#3344=PROPERTY_DEFINITION_REPRESENTATION(#3389,#3362);
#3345=PROPERTY_DEFINITION_REPRESENTATION(#3390,#3363);
#3346=PROPERTY_DEFINITION_REPRESENTATION(#3391,#3364);
#3347=PROPERTY_DEFINITION_REPRESENTATION(#3392,#3365);
#3348=PROPERTY_DEFINITION_REPRESENTATION(#3393,#3366);
#3349=PROPERTY_DEFINITION_REPRESENTATION(#3394,#3367);
#3350=PROPERTY_DEFINITION_REPRESENTATION(#3395,#3368);
#3351=PROPERTY_DEFINITION_REPRESENTATION(#3396,#3369);
#3352=REPRESENTATION('material name',(#3370),#9813);
#3353=REPRESENTATION('density',(#3325),#9813);
#3354=REPRESENTATION('material name',(#3371),#9814);
#3355=REPRESENTATION('density',(#3326),#9814);
#3356=REPRESENTATION('material name',(#3372),#9815);
#3357=REPRESENTATION('density',(#3327),#9815);
#3358=REPRESENTATION('material name',(#3373),#9816);
#3359=REPRESENTATION('density',(#3328),#9816);
#3360=REPRESENTATION('material name',(#3374),#9817);
#3361=REPRESENTATION('density',(#3329),#9817);
#3362=REPRESENTATION('material name',(#3375),#9818);
#3363=REPRESENTATION('density',(#3330),#9818);
#3364=REPRESENTATION('material name',(#3376),#9819);
#3365=REPRESENTATION('density',(#3331),#9819);
#3366=REPRESENTATION('material name',(#3377),#9820);
#3367=REPRESENTATION('density',(#3332),#9820);
#3368=REPRESENTATION('material name',(#3378),#9821);
#3369=REPRESENTATION('density',(#3333),#9821);
#3370=DESCRIPTIVE_REPRESENTATION_ITEM('Steel','Steel');
#3371=DESCRIPTIVE_REPRESENTATION_ITEM('Steel','Steel');
#3372=DESCRIPTIVE_REPRESENTATION_ITEM('Steel','Steel');
#3373=DESCRIPTIVE_REPRESENTATION_ITEM('Steel','Steel');
#3374=DESCRIPTIVE_REPRESENTATION_ITEM('Steel','Steel');
#3375=DESCRIPTIVE_REPRESENTATION_ITEM('Steel','Steel');
#3376=DESCRIPTIVE_REPRESENTATION_ITEM('Steel','Steel');
#3377=DESCRIPTIVE_REPRESENTATION_ITEM('Steel','Steel');
#3378=DESCRIPTIVE_REPRESENTATION_ITEM('Steel','Steel');
#3379=PROPERTY_DEFINITION('material property','material name',#9868);
#3380=PROPERTY_DEFINITION('material property','density of part',#9868);
#3381=PROPERTY_DEFINITION('material property','material name',#9869);
#3382=PROPERTY_DEFINITION('material property','density of part',#9869);
#3383=PROPERTY_DEFINITION('material property','material name',#9870);
#3384=PROPERTY_DEFINITION('material property','density of part',#9870);
#3385=PROPERTY_DEFINITION('material property','material name',#9871);
#3386=PROPERTY_DEFINITION('material property','density of part',#9871);
#3387=PROPERTY_DEFINITION('material property','material name',#9872);
#3388=PROPERTY_DEFINITION('material property','density of part',#9872);
#3389=PROPERTY_DEFINITION('material property','material name',#9873);
#3390=PROPERTY_DEFINITION('material property','density of part',#9873);
#3391=PROPERTY_DEFINITION('material property','material name',#9874);
#3392=PROPERTY_DEFINITION('material property','density of part',#9874);
#3393=PROPERTY_DEFINITION('material property','material name',#9875);
#3394=PROPERTY_DEFINITION('material property','density of part',#9875);
#3395=PROPERTY_DEFINITION('material property','material name',#9876);
#3396=PROPERTY_DEFINITION('material property','density of part',#9876);
#3397=AXIS2_PLACEMENT_3D('',#4646,#3727,#3728);
#3398=AXIS2_PLACEMENT_3D('',#4647,#3729,#3730);
#3399=AXIS2_PLACEMENT_3D('',#4648,#3731,#3732);
#3400=AXIS2_PLACEMENT_3D('',#4651,#3733,#3734);
#3401=AXIS2_PLACEMENT_3D('',#4655,#3736,#3737);
#3402=AXIS2_PLACEMENT_3D('',#4657,#3739,#3740);
#3403=AXIS2_PLACEMENT_3D('',#4663,#3744,#3745);
#3404=AXIS2_PLACEMENT_3D('',#4666,#3746,#3747);
#3405=AXIS2_PLACEMENT_3D('',#4670,#3749,#3750);
#3406=AXIS2_PLACEMENT_3D('',#4672,#3752,#3753);
#3407=AXIS2_PLACEMENT_3D('',#4678,#3757,#3758);
#3408=AXIS2_PLACEMENT_3D('',#4681,#3759,#3760);
#3409=AXIS2_PLACEMENT_3D('',#4685,#3762,#3763);
#3410=AXIS2_PLACEMENT_3D('',#4687,#3765,#3766);
#3411=AXIS2_PLACEMENT_3D('',#4693,#3770,#3771);
#3412=AXIS2_PLACEMENT_3D('',#4696,#3772,#3773);
#3413=AXIS2_PLACEMENT_3D('',#4700,#3775,#3776);
#3414=AXIS2_PLACEMENT_3D('',#4702,#3778,#3779);
#3415=AXIS2_PLACEMENT_3D('',#4708,#3783,#3784);
#3416=AXIS2_PLACEMENT_3D('',#4711,#3785,#3786);
#3417=AXIS2_PLACEMENT_3D('',#4715,#3788,#3789);
#3418=AXIS2_PLACEMENT_3D('',#4717,#3791,#3792);
#3419=AXIS2_PLACEMENT_3D('',#4723,#3796,#3797);
#3420=AXIS2_PLACEMENT_3D('',#4726,#3798,#3799);
#3421=AXIS2_PLACEMENT_3D('',#4730,#3801,#3802);
#3422=AXIS2_PLACEMENT_3D('',#4732,#3804,#3805);
#3423=AXIS2_PLACEMENT_3D('',#4738,#3809,#3810);
#3424=AXIS2_PLACEMENT_3D('',#4741,#3811,#3812);
#3425=AXIS2_PLACEMENT_3D('',#4745,#3814,#3815);
#3426=AXIS2_PLACEMENT_3D('',#4747,#3817,#3818);
#3427=AXIS2_PLACEMENT_3D('',#4753,#3822,#3823);
#3428=AXIS2_PLACEMENT_3D('',#4756,#3824,#3825);
#3429=AXIS2_PLACEMENT_3D('',#4760,#3827,#3828);
#3430=AXIS2_PLACEMENT_3D('',#4762,#3830,#3831);
#3431=AXIS2_PLACEMENT_3D('',#4768,#3835,#3836);
#3432=AXIS2_PLACEMENT_3D('',#4771,#3837,#3838);
#3433=AXIS2_PLACEMENT_3D('',#4775,#3840,#3841);
#3434=AXIS2_PLACEMENT_3D('',#4777,#3843,#3844);
#3435=AXIS2_PLACEMENT_3D('',#4783,#3848,#3849);
#3436=AXIS2_PLACEMENT_3D('',#4786,#3850,#3851);
#3437=AXIS2_PLACEMENT_3D('',#4790,#3853,#3854);
#3438=AXIS2_PLACEMENT_3D('',#4792,#3856,#3857);
#3439=AXIS2_PLACEMENT_3D('',#5101,#3862,#3863);
#3440=AXIS2_PLACEMENT_3D('',#5103,#3864,#3865);
#3441=AXIS2_PLACEMENT_3D('',#5105,#3866,#3867);
#3442=AXIS2_PLACEMENT_3D('',#5710,#3870,#3871);
#3443=AXIS2_PLACEMENT_3D('',#5712,#3872,#3873);
#3444=AXIS2_PLACEMENT_3D('',#5714,#3874,#3875);
#3445=AXIS2_PLACEMENT_3D('',#6319,#3878,#3879);
#3446=AXIS2_PLACEMENT_3D('',#6321,#3880,#3881);
#3447=AXIS2_PLACEMENT_3D('',#6323,#3882,#3883);
#3448=AXIS2_PLACEMENT_3D('',#6928,#3886,#3887);
#3449=AXIS2_PLACEMENT_3D('',#6930,#3888,#3889);
#3450=AXIS2_PLACEMENT_3D('',#6932,#3890,#3891);
#3451=AXIS2_PLACEMENT_3D('',#7537,#3894,#3895);
#3452=AXIS2_PLACEMENT_3D('',#7539,#3896,#3897);
#3453=AXIS2_PLACEMENT_3D('',#7541,#3898,#3899);
#3454=AXIS2_PLACEMENT_3D('',#7843,#3901,#3902);
#3455=AXIS2_PLACEMENT_3D('',#7844,#3903,#3904);
#3456=AXIS2_PLACEMENT_3D('',#7845,#3905,#3906);
#3457=AXIS2_PLACEMENT_3D('',#7846,#3907,#3908);
#3458=AXIS2_PLACEMENT_3D('',#7848,#3909,#3910);
#3459=AXIS2_PLACEMENT_3D('',#7850,#3911,#3912);
#3460=AXIS2_PLACEMENT_3D('',#7930,#3914,#3915);
#3461=AXIS2_PLACEMENT_3D('',#8010,#3917,#3918);
#3462=AXIS2_PLACEMENT_3D('',#8011,#3919,#3920);
#3463=AXIS2_PLACEMENT_3D('',#8012,#3921,#3922);
#3464=AXIS2_PLACEMENT_3D('',#8014,#3923,#3924);
#3465=AXIS2_PLACEMENT_3D('',#8015,#3925,#3926);
#3466=AXIS2_PLACEMENT_3D('',#8017,#3927,#3928);
#3467=AXIS2_PLACEMENT_3D('',#8019,#3930,#3931);
#3468=AXIS2_PLACEMENT_3D('',#8020,#3932,#3933);
#3469=AXIS2_PLACEMENT_3D('',#8021,#3934,#3935);
#3470=AXIS2_PLACEMENT_3D('',#8022,#3936,#3937);
#3471=AXIS2_PLACEMENT_3D('',#8023,#3938,#3939);
#3472=AXIS2_PLACEMENT_3D('',#8024,#3940,#3941);
#3473=AXIS2_PLACEMENT_3D('',#8025,#3942,#3943);
#3474=AXIS2_PLACEMENT_3D('',#8026,#3944,#3945);
#3475=AXIS2_PLACEMENT_3D('',#8027,#3946,#3947);
#3476=AXIS2_PLACEMENT_3D('',#8029,#3948,#3949);
#3477=AXIS2_PLACEMENT_3D('',#8031,#3951,#3952);
#3478=AXIS2_PLACEMENT_3D('',#8035,#3955,#3956);
#3479=AXIS2_PLACEMENT_3D('',#8039,#3958,#3959);
#3480=AXIS2_PLACEMENT_3D('',#8041,#3961,#3962);
#3481=AXIS2_PLACEMENT_3D('',#8272,#3966,#3967);
#3482=AXIS2_PLACEMENT_3D('',#8274,#3968,#3969);
#3483=AXIS2_PLACEMENT_3D('',#8501,#3971,#3972);
#3484=AXIS2_PLACEMENT_3D('',#8502,#3973,#3974);
#3485=AXIS2_PLACEMENT_3D('',#8504,#3975,#3976);
#3486=AXIS2_PLACEMENT_3D('',#8505,#3977,#3978);
#3487=AXIS2_PLACEMENT_3D('',#8507,#3980,#3981);
#3488=AXIS2_PLACEMENT_3D('',#8508,#3982,#3983);
#3489=AXIS2_PLACEMENT_3D('',#8509,#3984,#3985);
#3490=AXIS2_PLACEMENT_3D('',#8512,#3986,#3987);
#3491=AXIS2_PLACEMENT_3D('',#8513,#3988,#3989);
#3492=AXIS2_PLACEMENT_3D('',#8553,#3991,#3992);
#3493=AXIS2_PLACEMENT_3D('',#8557,#3994,#3995);
#3494=AXIS2_PLACEMENT_3D('',#8559,#3997,#3998);
#3495=AXIS2_PLACEMENT_3D('',#8565,#4002,#4003);
#3496=AXIS2_PLACEMENT_3D('',#8588,#4006,#4007);
#3497=AXIS2_PLACEMENT_3D('',#8592,#4010,#4011);
#3498=AXIS2_PLACEMENT_3D('',#8596,#4014,#4015);
#3499=AXIS2_PLACEMENT_3D('',#8598,#4016,#4017);
#3500=AXIS2_PLACEMENT_3D('',#8601,#4019,#4020);
#3501=AXIS2_PLACEMENT_3D('',#8602,#4021,#4022);
#3502=AXIS2_PLACEMENT_3D('',#8603,#4023,#4024);
#3503=AXIS2_PLACEMENT_3D('',#8608,#4026,#4027);
#3504=AXIS2_PLACEMENT_3D('',#8611,#4029,#4030);
#3505=AXIS2_PLACEMENT_3D('',#8612,#4031,#4032);
#3506=AXIS2_PLACEMENT_3D('',#8617,#4034,#4035);
#3507=AXIS2_PLACEMENT_3D('',#8620,#4037,#4038);
#3508=AXIS2_PLACEMENT_3D('',#8621,#4039,#4040);
#3509=AXIS2_PLACEMENT_3D('',#8626,#4042,#4043);
#3510=AXIS2_PLACEMENT_3D('',#8629,#4045,#4046);
#3511=AXIS2_PLACEMENT_3D('',#8630,#4047,#4048);
#3512=AXIS2_PLACEMENT_3D('',#8632,#4049,#4050);
#3513=AXIS2_PLACEMENT_3D('',#8633,#4051,#4052);
#3514=AXIS2_PLACEMENT_3D('',#8634,#4053,#4054);
#3515=AXIS2_PLACEMENT_3D('',#8635,#4055,#4056);
#3516=AXIS2_PLACEMENT_3D('',#8636,#4057,#4058);
#3517=AXIS2_PLACEMENT_3D('',#8640,#4060,#4061);
#3518=AXIS2_PLACEMENT_3D('',#8642,#4063,#4064);
#3519=AXIS2_PLACEMENT_3D('',#8646,#4066,#4067);
#3520=AXIS2_PLACEMENT_3D('',#8648,#4069,#4070);
#3521=AXIS2_PLACEMENT_3D('',#8663,#4072,#4073);
#3522=AXIS2_PLACEMENT_3D('',#8665,#4074,#4075);
#3523=AXIS2_PLACEMENT_3D('',#8667,#4076,#4077);
#3524=AXIS2_PLACEMENT_3D('',#8694,#4080,#4081);
#3525=AXIS2_PLACEMENT_3D('',#8696,#4082,#4083);
#3526=AXIS2_PLACEMENT_3D('',#8698,#4084,#4085);
#3527=AXIS2_PLACEMENT_3D('',#8725,#4088,#4089);
#3528=AXIS2_PLACEMENT_3D('',#8727,#4090,#4091);
#3529=AXIS2_PLACEMENT_3D('',#8729,#4092,#4093);
#3530=AXIS2_PLACEMENT_3D('',#8742,#4095,#4096);
#3531=AXIS2_PLACEMENT_3D('',#8744,#4097,#4098);
#3532=AXIS2_PLACEMENT_3D('',#8747,#4100,#4101);
#3533=AXIS2_PLACEMENT_3D('',#8748,#4102,#4103);
#3534=AXIS2_PLACEMENT_3D('',#8749,#4104,#4105);
#3535=AXIS2_PLACEMENT_3D('',#8751,#4106,#4107);
#3536=AXIS2_PLACEMENT_3D('',#8753,#4109,#4110);
#3537=AXIS2_PLACEMENT_3D('',#8754,#4111,#4112);
#3538=AXIS2_PLACEMENT_3D('',#8758,#4114,#4115);
#3539=AXIS2_PLACEMENT_3D('',#8760,#4117,#4118);
#3540=AXIS2_PLACEMENT_3D('',#8762,#4119,#4120);
#3541=AXIS2_PLACEMENT_3D('',#8764,#4122,#4123);
#3542=AXIS2_PLACEMENT_3D('',#8830,#4127,#4128);
#3543=AXIS2_PLACEMENT_3D('',#8834,#4131,#4132);
#3544=AXIS2_PLACEMENT_3D('',#8835,#4133,#4134);
#3545=AXIS2_PLACEMENT_3D('',#8836,#4135,#4136);
#3546=AXIS2_PLACEMENT_3D('',#8837,#4137,#4138);
#3547=AXIS2_PLACEMENT_3D('',#8841,#4140,#4141);
#3548=AXIS2_PLACEMENT_3D('',#8843,#4143,#4144);
#3549=AXIS2_PLACEMENT_3D('',#8845,#4145,#4146);
#3550=AXIS2_PLACEMENT_3D('',#8847,#4148,#4149);
#3551=AXIS2_PLACEMENT_3D('',#8913,#4153,#4154);
#3552=AXIS2_PLACEMENT_3D('',#8917,#4157,#4158);
#3553=AXIS2_PLACEMENT_3D('',#8918,#4159,#4160);
#3554=AXIS2_PLACEMENT_3D('',#8919,#4161,#4162);
#3555=AXIS2_PLACEMENT_3D('',#8920,#4163,#4164);
#3556=AXIS2_PLACEMENT_3D('',#8924,#4166,#4167);
#3557=AXIS2_PLACEMENT_3D('',#8926,#4169,#4170);
#3558=AXIS2_PLACEMENT_3D('',#8928,#4171,#4172);
#3559=AXIS2_PLACEMENT_3D('',#8930,#4174,#4175);
#3560=AXIS2_PLACEMENT_3D('',#8966,#4179,#4180);
#3561=AXIS2_PLACEMENT_3D('',#8968,#4181,#4182);
#3562=AXIS2_PLACEMENT_3D('',#9002,#4185,#4186);
#3563=AXIS2_PLACEMENT_3D('',#9006,#4189,#4190);
#3564=AXIS2_PLACEMENT_3D('',#9007,#4191,#4192);
#3565=AXIS2_PLACEMENT_3D('',#9008,#4193,#4194);
#3566=AXIS2_PLACEMENT_3D('',#9009,#4195,#4196);
#3567=AXIS2_PLACEMENT_3D('',#9010,#4197,#4198);
#3568=AXIS2_PLACEMENT_3D('',#9013,#4199,#4200);
#3569=AXIS2_PLACEMENT_3D('',#9014,#4201,#4202);
#3570=AXIS2_PLACEMENT_3D('',#9054,#4204,#4205);
#3571=AXIS2_PLACEMENT_3D('',#9060,#4209,#4210);
#3572=AXIS2_PLACEMENT_3D('',#9064,#4212,#4213);
#3573=AXIS2_PLACEMENT_3D('',#9066,#4215,#4216);
#3574=AXIS2_PLACEMENT_3D('',#9072,#4220,#4221);
#3575=AXIS2_PLACEMENT_3D('',#9093,#4223,#4224);
#3576=AXIS2_PLACEMENT_3D('',#9097,#4227,#4228);
#3577=AXIS2_PLACEMENT_3D('',#9099,#4229,#4230);
#3578=AXIS2_PLACEMENT_3D('',#9102,#4232,#4233);
#3579=AXIS2_PLACEMENT_3D('',#9103,#4234,#4235);
#3580=AXIS2_PLACEMENT_3D('',#9104,#4236,#4237);
#3581=AXIS2_PLACEMENT_3D('',#9109,#4239,#4240);
#3582=AXIS2_PLACEMENT_3D('',#9112,#4242,#4243);
#3583=AXIS2_PLACEMENT_3D('',#9113,#4244,#4245);
#3584=AXIS2_PLACEMENT_3D('',#9118,#4247,#4248);
#3585=AXIS2_PLACEMENT_3D('',#9121,#4250,#4251);
#3586=AXIS2_PLACEMENT_3D('',#9122,#4252,#4253);
#3587=AXIS2_PLACEMENT_3D('',#9127,#4255,#4256);
#3588=AXIS2_PLACEMENT_3D('',#9130,#4258,#4259);
#3589=AXIS2_PLACEMENT_3D('',#9131,#4260,#4261);
#3590=AXIS2_PLACEMENT_3D('',#9133,#4262,#4263);
#3591=AXIS2_PLACEMENT_3D('',#9134,#4264,#4265);
#3592=AXIS2_PLACEMENT_3D('',#9135,#4266,#4267);
#3593=AXIS2_PLACEMENT_3D('',#9136,#4268,#4269);
#3594=AXIS2_PLACEMENT_3D('',#9137,#4270,#4271);
#3595=AXIS2_PLACEMENT_3D('',#9141,#4273,#4274);
#3596=AXIS2_PLACEMENT_3D('',#9143,#4276,#4277);
#3597=AXIS2_PLACEMENT_3D('',#9147,#4279,#4280);
#3598=AXIS2_PLACEMENT_3D('',#9149,#4282,#4283);
#3599=AXIS2_PLACEMENT_3D('',#9164,#4285,#4286);
#3600=AXIS2_PLACEMENT_3D('',#9166,#4287,#4288);
#3601=AXIS2_PLACEMENT_3D('',#9168,#4289,#4290);
#3602=AXIS2_PLACEMENT_3D('',#9195,#4293,#4294);
#3603=AXIS2_PLACEMENT_3D('',#9197,#4295,#4296);
#3604=AXIS2_PLACEMENT_3D('',#9199,#4297,#4298);
#3605=AXIS2_PLACEMENT_3D('',#9226,#4301,#4302);
#3606=AXIS2_PLACEMENT_3D('',#9228,#4303,#4304);
#3607=AXIS2_PLACEMENT_3D('',#9230,#4305,#4306);
#3608=AXIS2_PLACEMENT_3D('',#9243,#4308,#4309);
#3609=AXIS2_PLACEMENT_3D('',#9245,#4310,#4311);
#3610=AXIS2_PLACEMENT_3D('',#9248,#4313,#4314);
#3611=AXIS2_PLACEMENT_3D('',#9249,#4315,#4316);
#3612=AXIS2_PLACEMENT_3D('',#9250,#4317,#4318);
#3613=AXIS2_PLACEMENT_3D('',#9253,#4320,#4321);
#3614=AXIS2_PLACEMENT_3D('',#9254,#4322,#4323);
#3615=AXIS2_PLACEMENT_3D('',#9255,#4324,#4325);
#3616=AXIS2_PLACEMENT_3D('',#9259,#4327,#4328);
#3617=AXIS2_PLACEMENT_3D('',#9261,#4330,#4331);
#3618=AXIS2_PLACEMENT_3D('',#9264,#4333,#4334);
#3619=AXIS2_PLACEMENT_3D('',#9265,#4335,#4336);
#3620=AXIS2_PLACEMENT_3D('',#9331,#4340,#4341);
#3621=AXIS2_PLACEMENT_3D('',#9335,#4344,#4345);
#3622=AXIS2_PLACEMENT_3D('',#9336,#4346,#4347);
#3623=AXIS2_PLACEMENT_3D('',#9337,#4348,#4349);
#3624=AXIS2_PLACEMENT_3D('',#9338,#4350,#4351);
#3625=AXIS2_PLACEMENT_3D('',#9342,#4353,#4354);
#3626=AXIS2_PLACEMENT_3D('',#9344,#4356,#4357);
#3627=AXIS2_PLACEMENT_3D('',#9347,#4359,#4360);
#3628=AXIS2_PLACEMENT_3D('',#9348,#4361,#4362);
#3629=AXIS2_PLACEMENT_3D('',#9414,#4366,#4367);
#3630=AXIS2_PLACEMENT_3D('',#9418,#4370,#4371);
#3631=AXIS2_PLACEMENT_3D('',#9419,#4372,#4373);
#3632=AXIS2_PLACEMENT_3D('',#9420,#4374,#4375);
#3633=AXIS2_PLACEMENT_3D('',#9421,#4376,#4377);
#3634=AXIS2_PLACEMENT_3D('',#9425,#4379,#4380);
#3635=AXIS2_PLACEMENT_3D('',#9427,#4382,#4383);
#3636=AXIS2_PLACEMENT_3D('',#9430,#4385,#4386);
#3637=AXIS2_PLACEMENT_3D('',#9431,#4387,#4388);
#3638=AXIS2_PLACEMENT_3D('',#9467,#4392,#4393);
#3639=AXIS2_PLACEMENT_3D('',#9470,#4395,#4396);
#3640=AXIS2_PLACEMENT_3D('',#9503,#4398,#4399);
#3641=AXIS2_PLACEMENT_3D('',#9507,#4402,#4403);
#3642=AXIS2_PLACEMENT_3D('',#9508,#4404,#4405);
#3643=AXIS2_PLACEMENT_3D('',#9509,#4406,#4407);
#3644=AXIS2_PLACEMENT_3D('',#9510,#4408,#4409);
#3645=AXIS2_PLACEMENT_3D('',#9511,#4410,#4411);
#3646=AXIS2_PLACEMENT_3D('',#9520,#4416,#4417);
#3647=AXIS2_PLACEMENT_3D('',#9526,#4421,#4422);
#3648=AXIS2_PLACEMENT_3D('',#9532,#4426,#4427);
#3649=AXIS2_PLACEMENT_3D('',#9538,#4431,#4432);
#3650=AXIS2_PLACEMENT_3D('',#9544,#4436,#4437);
#3651=AXIS2_PLACEMENT_3D('',#9547,#4440,#4441);
#3652=AXIS2_PLACEMENT_3D('',#9548,#4442,#4443);
#3653=AXIS2_PLACEMENT_3D('',#9550,#4444,#4445);
#3654=AXIS2_PLACEMENT_3D('',#9553,#4447,#4448);
#3655=AXIS2_PLACEMENT_3D('',#9554,#4449,#4450);
#3656=AXIS2_PLACEMENT_3D('',#9555,#4451,#4452);
#3657=AXIS2_PLACEMENT_3D('',#9556,#4453,#4454);
#3658=AXIS2_PLACEMENT_3D('',#9557,#4455,#4456);
#3659=AXIS2_PLACEMENT_3D('',#9566,#4461,#4462);
#3660=AXIS2_PLACEMENT_3D('',#9572,#4466,#4467);
#3661=AXIS2_PLACEMENT_3D('',#9578,#4471,#4472);
#3662=AXIS2_PLACEMENT_3D('',#9584,#4476,#4477);
#3663=AXIS2_PLACEMENT_3D('',#9590,#4481,#4482);
#3664=AXIS2_PLACEMENT_3D('',#9593,#4485,#4486);
#3665=AXIS2_PLACEMENT_3D('',#9594,#4487,#4488);
#3666=AXIS2_PLACEMENT_3D('',#9596,#4489,#4490);
#3667=AXIS2_PLACEMENT_3D('',#9599,#4492,#4493);
#3668=AXIS2_PLACEMENT_3D('',#9600,#4494,#4495);
#3669=AXIS2_PLACEMENT_3D('',#9601,#4496,#4497);
#3670=AXIS2_PLACEMENT_3D('',#9602,#4498,#4499);
#3671=AXIS2_PLACEMENT_3D('',#9603,#4500,#4501);
#3672=AXIS2_PLACEMENT_3D('',#9612,#4506,#4507);
#3673=AXIS2_PLACEMENT_3D('',#9633,#4508,#4509);
#3674=AXIS2_PLACEMENT_3D('',#9635,#4511,#4512);
#3675=AXIS2_PLACEMENT_3D('',#9637,#4513,#4514);
#3676=AXIS2_PLACEMENT_3D('',#9639,#4516,#4517);
#3677=AXIS2_PLACEMENT_3D('',#9643,#4520,#4521);
#3678=AXIS2_PLACEMENT_3D('',#9662,#4522,#4523);
#3679=AXIS2_PLACEMENT_3D('',#9664,#4524,#4525);
#3680=AXIS2_PLACEMENT_3D('',#9665,#4526,#4527);
#3681=AXIS2_PLACEMENT_3D('',#9667,#4528,#4529);
#3682=AXIS2_PLACEMENT_3D('',#9669,#4531,#4532);
#3683=AXIS2_PLACEMENT_3D('',#9670,#4533,#4534);
#3684=AXIS2_PLACEMENT_3D('',#9671,#4535,#4536);
#3685=AXIS2_PLACEMENT_3D('',#9680,#4541,#4542);
#3686=AXIS2_PLACEMENT_3D('',#9702,#4544,#4545);
#3687=AXIS2_PLACEMENT_3D('',#9703,#4546,#4547);
#3688=AXIS2_PLACEMENT_3D('',#9706,#4549,#4550);
#3689=AXIS2_PLACEMENT_3D('',#9707,#4551,#4552);
#3690=AXIS2_PLACEMENT_3D('',#9711,#4555,#4556);
#3691=AXIS2_PLACEMENT_3D('',#9730,#4557,#4558);
#3692=AXIS2_PLACEMENT_3D('',#9732,#4559,#4560);
#3693=AXIS2_PLACEMENT_3D('',#9733,#4561,#4562);
#3694=AXIS2_PLACEMENT_3D('',#9736,#4564,#4565);
#3695=AXIS2_PLACEMENT_3D('',#9737,#4566,#4567);
#3696=AXIS2_PLACEMENT_3D('',#9738,#4568,#4569);
#3697=AXIS2_PLACEMENT_3D('',#9739,#4570,#4571);
#3698=AXIS2_PLACEMENT_3D('',#9742,#4572,#4573);
#3699=AXIS2_PLACEMENT_3D('',#9746,#4575,#4576);
#3700=AXIS2_PLACEMENT_3D('',#9748,#4578,#4579);
#3701=AXIS2_PLACEMENT_3D('',#9754,#4583,#4584);
#3702=AXIS2_PLACEMENT_3D('',#9756,#4585,#4586);
#3703=AXIS2_PLACEMENT_3D('',#9758,#4588,#4589);
#3704=AXIS2_PLACEMENT_3D('',#9761,#4591,#4592);
#3705=AXIS2_PLACEMENT_3D('',#9762,#4593,#4594);
#3706=AXIS2_PLACEMENT_3D('',#9764,#4596,#4597);
#3707=AXIS2_PLACEMENT_3D('',#9765,#4598,#4599);
#3708=AXIS2_PLACEMENT_3D('',#9766,#4600,#4601);
#3709=AXIS2_PLACEMENT_3D('',#9769,#4602,#4603);
#3710=AXIS2_PLACEMENT_3D('',#9773,#4605,#4606);
#3711=AXIS2_PLACEMENT_3D('',#9775,#4608,#4609);
#3712=AXIS2_PLACEMENT_3D('',#9781,#4613,#4614);
#3713=AXIS2_PLACEMENT_3D('',#9784,#4616,#4617);
#3714=AXIS2_PLACEMENT_3D('',#9785,#4618,#4619);
#3715=AXIS2_PLACEMENT_3D('',#9787,#4620,#4621);
#3716=AXIS2_PLACEMENT_3D('',#9789,#4623,#4624);
#3717=AXIS2_PLACEMENT_3D('',#9791,#4626,#4627);
#3718=AXIS2_PLACEMENT_3D('',#9792,#4628,#4629);
#3719=AXIS2_PLACEMENT_3D('',#9793,#4630,#4631);
#3720=AXIS2_PLACEMENT_3D('',#9794,#4632,#4633);
#3721=AXIS2_PLACEMENT_3D('',#9795,#4634,#4635);
#3722=AXIS2_PLACEMENT_3D('',#9796,#4636,#4637);
#3723=AXIS2_PLACEMENT_3D('',#9797,#4638,#4639);
#3724=AXIS2_PLACEMENT_3D('',#9798,#4640,#4641);
#3725=AXIS2_PLACEMENT_3D('',#9799,#4642,#4643);
#3726=AXIS2_PLACEMENT_3D('',#9800,#4644,#4645);
#3727=DIRECTION('axis',(0.,0.,1.));
#3728=DIRECTION('refdir',(1.,0.,0.));
#3729=DIRECTION('axis',(0.,0.,1.));
#3730=DIRECTION('refdir',(1.,0.,0.));
#3731=DIRECTION('center_axis',(0.,0.,-1.));
#3732=DIRECTION('ref_axis',(-0.995790400289429,-0.091659580467175,0.));
#3733=DIRECTION('center_axis',(0.,0.,-1.));
#3734=DIRECTION('ref_axis',(-0.995790400289429,-0.091659580467175,0.));
#3735=DIRECTION('',(0.,0.,-1.));
#3736=DIRECTION('center_axis',(0.,0.,-1.));
#3737=DIRECTION('ref_axis',(-0.995790400289429,-0.091659580467175,0.));
#3738=DIRECTION('',(0.,0.,1.));
#3739=DIRECTION('center_axis',(0.696489643340828,0.717566844774037,0.));
#3740=DIRECTION('ref_axis',(-0.717566844774037,0.696489643340828,0.));
#3741=DIRECTION('',(-0.717566844774037,0.696489643340828,0.));
#3742=DIRECTION('',(0.,0.,1.));
#3743=DIRECTION('',(-0.717566844774037,0.696489643340828,0.));
#3744=DIRECTION('center_axis',(0.,0.,1.));
#3745=DIRECTION('ref_axis',(0.577274725329514,0.816549993261732,0.));
#3746=DIRECTION('center_axis',(0.,0.,-1.));
#3747=DIRECTION('ref_axis',(0.577274725329514,0.816549993261732,0.));
#3748=DIRECTION('',(0.,0.,1.));
#3749=DIRECTION('center_axis',(0.,0.,-1.));
#3750=DIRECTION('ref_axis',(0.577274725329514,0.816549993261732,0.));
#3751=DIRECTION('',(0.,0.,-1.));
#3752=DIRECTION('center_axis',(-0.969675938158175,-0.2443943022189,0.));
#3753=DIRECTION('ref_axis',(0.2443943022189,-0.969675938158175,0.));
#3754=DIRECTION('',(0.2443943022189,-0.969675938158175,0.));
#3755=DIRECTION('',(0.,0.,1.));
#3756=DIRECTION('',(0.2443943022189,-0.969675938158175,0.));
#3757=DIRECTION('center_axis',(0.,0.,-1.));
#3758=DIRECTION('ref_axis',(-0.577274725329512,0.816549993261733,0.));
#3759=DIRECTION('center_axis',(0.,0.,-1.));
#3760=DIRECTION('ref_axis',(-0.577274725329512,0.816549993261733,0.));
#3761=DIRECTION('',(0.,0.,-1.));
#3762=DIRECTION('center_axis',(0.,0.,-1.));
#3763=DIRECTION('ref_axis',(-0.577274725329512,0.816549993261733,0.));
#3764=DIRECTION('',(0.,0.,1.));
#3765=DIRECTION('center_axis',(0.969675938158175,-0.244394302218901,0.));
#3766=DIRECTION('ref_axis',(0.244394302218901,0.969675938158175,0.));
#3767=DIRECTION('',(0.244394302218901,0.969675938158175,0.));
#3768=DIRECTION('',(0.,0.,1.));
#3769=DIRECTION('',(0.244394302218901,0.969675938158175,0.));
#3770=DIRECTION('center_axis',(0.,0.,1.));
#3771=DIRECTION('ref_axis',(0.995790400289429,-0.0916595804671751,0.));
#3772=DIRECTION('center_axis',(0.,0.,-1.));
#3773=DIRECTION('ref_axis',(0.995790400289429,-0.0916595804671751,0.));
#3774=DIRECTION('',(0.,0.,1.));
#3775=DIRECTION('center_axis',(0.,0.,-1.));
#3776=DIRECTION('ref_axis',(0.995790400289429,-0.0916595804671751,0.));
#3777=DIRECTION('',(0.,0.,-1.));
#3778=DIRECTION('center_axis',(-0.696489643340827,0.717566844774038,0.));
#3779=DIRECTION('ref_axis',(-0.717566844774038,-0.696489643340827,0.));
#3780=DIRECTION('',(-0.717566844774038,-0.696489643340827,0.));
#3781=DIRECTION('',(0.,0.,1.));
#3782=DIRECTION('',(-0.717566844774038,-0.696489643340827,0.));
#3783=DIRECTION('center_axis',(0.,0.,-1.));
#3784=DIRECTION('ref_axis',(0.418515674959917,0.908209573728908,0.));
#3785=DIRECTION('center_axis',(0.,0.,-1.));
#3786=DIRECTION('ref_axis',(0.418515674959917,0.908209573728908,0.));
#3787=DIRECTION('',(0.,0.,-1.));
#3788=DIRECTION('center_axis',(0.,0.,-1.));
#3789=DIRECTION('ref_axis',(0.418515674959917,0.908209573728908,0.));
#3790=DIRECTION('',(0.,0.,1.));
#3791=DIRECTION('center_axis',(0.273186294817348,-0.961961146992938,0.));
#3792=DIRECTION('ref_axis',(0.961961146992938,0.273186294817348,0.));
#3793=DIRECTION('',(0.961961146992938,0.273186294817348,0.));
#3794=DIRECTION('',(0.,0.,1.));
#3795=DIRECTION('',(0.961961146992938,0.273186294817348,0.));
#3796=DIRECTION('center_axis',(0.,0.,1.));
#3797=DIRECTION('ref_axis',(0.418515674959918,-0.908209573728908,0.));
#3798=DIRECTION('center_axis',(0.,0.,-1.));
#3799=DIRECTION('ref_axis',(0.418515674959918,-0.908209573728908,0.));
#3800=DIRECTION('',(0.,0.,1.));
#3801=DIRECTION('center_axis',(0.,0.,-1.));
#3802=DIRECTION('ref_axis',(0.418515674959918,-0.908209573728908,0.));
#3803=DIRECTION('',(0.,0.,-1.));
#3804=DIRECTION('center_axis',(0.273186294817348,0.961961146992938,0.));
#3805=DIRECTION('ref_axis',(-0.961961146992938,0.273186294817348,0.));
#3806=DIRECTION('',(-0.961961146992938,0.273186294817348,0.));
#3807=DIRECTION('',(0.,0.,1.));
#3808=DIRECTION('',(-0.961961146992938,0.273186294817348,0.));
#3809=DIRECTION('center_axis',(0.,0.,-1.));
#3810=DIRECTION('ref_axis',(0.995790400289429,0.0916595804671737,0.));
#3811=DIRECTION('center_axis',(0.,0.,-1.));
#3812=DIRECTION('ref_axis',(0.995790400289429,0.0916595804671737,0.));
#3813=DIRECTION('',(0.,0.,-1.));
#3814=DIRECTION('center_axis',(0.,0.,-1.));
#3815=DIRECTION('ref_axis',(0.995790400289429,0.0916595804671737,0.));
#3816=DIRECTION('',(0.,0.,1.));
#3817=DIRECTION('center_axis',(-0.696489643340827,-0.717566844774037,0.));
#3818=DIRECTION('ref_axis',(0.717566844774037,-0.696489643340827,0.));
#3819=DIRECTION('',(0.717566844774037,-0.696489643340827,0.));
#3820=DIRECTION('',(0.,0.,1.));
#3821=DIRECTION('',(0.717566844774037,-0.696489643340827,0.));
#3822=DIRECTION('center_axis',(0.,0.,1.));
#3823=DIRECTION('ref_axis',(-0.577274725329511,-0.816549993261734,0.));
#3824=DIRECTION('center_axis',(0.,0.,-1.));
#3825=DIRECTION('ref_axis',(-0.577274725329511,-0.816549993261734,0.));
#3826=DIRECTION('',(0.,0.,1.));
#3827=DIRECTION('center_axis',(0.,0.,-1.));
#3828=DIRECTION('ref_axis',(-0.577274725329511,-0.816549993261734,0.));
#3829=DIRECTION('',(0.,0.,-1.));
#3830=DIRECTION('center_axis',(0.969675938158175,0.244394302218901,0.));
#3831=DIRECTION('ref_axis',(-0.244394302218901,0.969675938158175,0.));
#3832=DIRECTION('',(-0.244394302218901,0.969675938158175,0.));
#3833=DIRECTION('',(0.,0.,1.));
#3834=DIRECTION('',(-0.244394302218901,0.969675938158175,0.));
#3835=DIRECTION('center_axis',(0.,0.,-1.));
#3836=DIRECTION('ref_axis',(0.577274725329512,-0.816549993261733,0.));
#3837=DIRECTION('center_axis',(0.,0.,-1.));
#3838=DIRECTION('ref_axis',(0.577274725329512,-0.816549993261733,0.));
#3839=DIRECTION('',(0.,0.,-1.));
#3840=DIRECTION('center_axis',(0.,0.,-1.));
#3841=DIRECTION('ref_axis',(0.577274725329512,-0.816549993261733,0.));
#3842=DIRECTION('',(0.,0.,1.));
#3843=DIRECTION('center_axis',(-0.969675938158175,0.244394302218901,0.));
#3844=DIRECTION('ref_axis',(-0.244394302218901,-0.969675938158175,0.));
#3845=DIRECTION('',(-0.244394302218901,-0.969675938158175,0.));
#3846=DIRECTION('',(0.,0.,1.));
#3847=DIRECTION('',(-0.244394302218901,-0.969675938158175,0.));
#3848=DIRECTION('center_axis',(0.,0.,1.));
#3849=DIRECTION('ref_axis',(-0.995790400289429,0.0916595804671751,0.));
#3850=DIRECTION('center_axis',(0.,0.,-1.));
#3851=DIRECTION('ref_axis',(-0.995790400289429,0.0916595804671751,0.));
#3852=DIRECTION('',(0.,0.,1.));
#3853=DIRECTION('center_axis',(0.,0.,-1.));
#3854=DIRECTION('ref_axis',(-0.995790400289429,0.0916595804671751,0.));
#3855=DIRECTION('',(0.,0.,-1.));
#3856=DIRECTION('center_axis',(0.696489643340827,-0.717566844774037,0.));
#3857=DIRECTION('ref_axis',(0.717566844774037,0.696489643340827,0.));
#3858=DIRECTION('',(0.717566844774037,0.696489643340827,0.));
#3859=DIRECTION('',(0.,0.,1.));
#3860=DIRECTION('',(0.717566844774037,0.696489643340827,0.));
#3861=DIRECTION('',(0.,0.,1.));
#3862=DIRECTION('center_axis',(0.,0.,1.));
#3863=DIRECTION('ref_axis',(0.448260781250512,-0.893902831404332,0.));
#3864=DIRECTION('center_axis',(0.,0.,1.));
#3865=DIRECTION('ref_axis',(0.448260781250512,-0.893902831404332,0.));
#3866=DIRECTION('center_axis',(0.,0.,1.));
#3867=DIRECTION('ref_axis',(0.448260781250512,-0.893902831404332,0.));
#3868=DIRECTION('',(0.,0.,1.));
#3869=DIRECTION('',(0.,0.,1.));
#3870=DIRECTION('center_axis',(0.,0.,1.));
#3871=DIRECTION('ref_axis',(-0.550012169885733,-0.835156639785368,0.));
#3872=DIRECTION('center_axis',(0.,0.,1.));
#3873=DIRECTION('ref_axis',(-0.550012169885733,-0.835156639785368,0.));
#3874=DIRECTION('center_axis',(0.,0.,1.));
#3875=DIRECTION('ref_axis',(-0.550012169885733,-0.835156639785368,0.));
#3876=DIRECTION('',(0.,0.,1.));
#3877=DIRECTION('',(0.,0.,1.));
#3878=DIRECTION('center_axis',(0.,0.,1.));
#3879=DIRECTION('ref_axis',(-0.998272951136245,0.0587461916189628,0.));
#3880=DIRECTION('center_axis',(0.,0.,1.));
#3881=DIRECTION('ref_axis',(-0.998272951136245,0.0587461916189628,0.));
#3882=DIRECTION('center_axis',(0.,0.,1.));
#3883=DIRECTION('ref_axis',(-0.998272951136245,0.0587461916189628,0.));
#3884=DIRECTION('',(0.,0.,1.));
#3885=DIRECTION('',(0.,0.,1.));
#3886=DIRECTION('center_axis',(0.,0.,1.));
#3887=DIRECTION('ref_axis',(-0.448260781250512,0.893902831404331,0.));
#3888=DIRECTION('center_axis',(0.,0.,1.));
#3889=DIRECTION('ref_axis',(-0.448260781250512,0.893902831404331,0.));
#3890=DIRECTION('center_axis',(0.,0.,1.));
#3891=DIRECTION('ref_axis',(-0.448260781250512,0.893902831404331,0.));
#3892=DIRECTION('',(0.,0.,1.));
#3893=DIRECTION('',(0.,0.,1.));
#3894=DIRECTION('center_axis',(0.,0.,1.));
#3895=DIRECTION('ref_axis',(0.550012169885733,0.835156639785369,0.));
#3896=DIRECTION('center_axis',(0.,0.,1.));
#3897=DIRECTION('ref_axis',(0.550012169885733,0.835156639785369,0.));
#3898=DIRECTION('center_axis',(0.,0.,1.));
#3899=DIRECTION('ref_axis',(0.550012169885733,0.835156639785369,0.));
#3900=DIRECTION('',(0.,0.,1.));
#3901=DIRECTION('center_axis',(0.,0.,1.));
#3902=DIRECTION('ref_axis',(1.,0.,0.));
#3903=DIRECTION('center_axis',(0.,0.,1.));
#3904=DIRECTION('ref_axis',(1.,0.,0.));
#3905=DIRECTION('center_axis',(0.,0.,1.));
#3906=DIRECTION('ref_axis',(1.,0.,0.));
#3907=DIRECTION('center_axis',(0.,0.,1.));
#3908=DIRECTION('ref_axis',(1.,0.,0.));
#3909=DIRECTION('center_axis',(0.,0.,1.));
#3910=DIRECTION('ref_axis',(1.,0.,0.));
#3911=DIRECTION('center_axis',(0.,0.,-1.));
#3912=DIRECTION('ref_axis',(-0.418515674959917,-0.908209573728908,0.));
#3913=DIRECTION('',(-0.961961146992938,-0.273186294817348,0.));
#3914=DIRECTION('center_axis',(0.,0.,1.));
#3915=DIRECTION('ref_axis',(0.998272951136245,-0.0587461916189627,0.));
#3916=DIRECTION('',(0.961961146992938,-0.273186294817348,0.));
#3917=DIRECTION('center_axis',(0.,0.,-1.));
#3918=DIRECTION('ref_axis',(-0.418515674959917,0.908209573728908,0.));
#3919=DIRECTION('center_axis',(0.,0.,1.));
#3920=DIRECTION('ref_axis',(1.,0.,0.));
#3921=DIRECTION('center_axis',(0.,0.,1.));
#3922=DIRECTION('ref_axis',(1.,0.,0.));
#3923=DIRECTION('center_axis',(0.,0.,-1.));
#3924=DIRECTION('ref_axis',(1.,0.,0.));
#3925=DIRECTION('center_axis',(0.,0.,1.));
#3926=DIRECTION('ref_axis',(1.,0.,0.));
#3927=DIRECTION('center_axis',(0.,0.,1.));
#3928=DIRECTION('ref_axis',(1.,0.,0.));
#3929=DIRECTION('',(0.,0.,1.));
#3930=DIRECTION('center_axis',(0.,0.,1.));
#3931=DIRECTION('ref_axis',(1.,0.,0.));
#3932=DIRECTION('center_axis',(0.,0.,1.));
#3933=DIRECTION('ref_axis',(1.,0.,0.));
#3934=DIRECTION('center_axis',(0.,0.,1.));
#3935=DIRECTION('ref_axis',(1.,0.,0.));
#3936=DIRECTION('center_axis',(0.,0.,1.));
#3937=DIRECTION('ref_axis',(1.,0.,0.));
#3938=DIRECTION('center_axis',(0.,0.,1.));
#3939=DIRECTION('ref_axis',(1.,0.,0.));
#3940=DIRECTION('center_axis',(0.,0.,1.));
#3941=DIRECTION('ref_axis',(1.,0.,0.));
#3942=DIRECTION('center_axis',(0.,0.,1.));
#3943=DIRECTION('ref_axis',(1.,0.,0.));
#3944=DIRECTION('center_axis',(0.,0.,1.));
#3945=DIRECTION('ref_axis',(1.,0.,0.));
#3946=DIRECTION('center_axis',(0.,0.,-1.));
#3947=DIRECTION('ref_axis',(-0.418515674959917,-0.908209573728908,0.));
#3948=DIRECTION('center_axis',(0.,0.,-1.));
#3949=DIRECTION('ref_axis',(-0.418515674959917,-0.908209573728908,0.));
#3950=DIRECTION('',(0.,0.,-1.));
#3951=DIRECTION('center_axis',(-0.273186294817348,0.961961146992938,0.));
#3952=DIRECTION('ref_axis',(-0.961961146992938,-0.273186294817348,0.));
#3953=DIRECTION('',(-0.961961146992938,-0.273186294817348,0.));
#3954=DIRECTION('',(0.,0.,1.));
#3955=DIRECTION('center_axis',(0.,0.,1.));
#3956=DIRECTION('ref_axis',(-0.418515674959917,0.908209573728908,0.));
#3957=DIRECTION('',(0.,0.,1.));
#3958=DIRECTION('center_axis',(0.,0.,-1.));
#3959=DIRECTION('ref_axis',(-0.418515674959917,0.908209573728908,0.));
#3960=DIRECTION('',(0.,0.,-1.));
#3961=DIRECTION('center_axis',(-0.273186294817348,-0.961961146992938,0.));
#3962=DIRECTION('ref_axis',(0.961961146992938,-0.273186294817348,0.));
#3963=DIRECTION('',(0.,0.,1.));
#3964=DIRECTION('',(0.961961146992938,-0.273186294817348,0.));
#3965=DIRECTION('',(0.,0.,1.));
#3966=DIRECTION('center_axis',(0.,0.,1.));
#3967=DIRECTION('ref_axis',(0.998272951136245,-0.0587461916189627,0.));
#3968=DIRECTION('center_axis',(0.,0.,1.));
#3969=DIRECTION('ref_axis',(0.998272951136245,-0.0587461916189627,0.));
#3970=DIRECTION('',(0.,0.,1.));
#3971=DIRECTION('center_axis',(0.,0.,1.));
#3972=DIRECTION('ref_axis',(1.,0.,0.));
#3973=DIRECTION('center_axis',(0.,0.,1.));
#3974=DIRECTION('ref_axis',(1.,0.,0.));
#3975=DIRECTION('center_axis',(0.,0.,-1.));
#3976=DIRECTION('ref_axis',(1.,0.,0.));
#3977=DIRECTION('center_axis',(0.,0.,1.));
#3978=DIRECTION('ref_axis',(1.,0.,0.));
#3979=DIRECTION('',(0.,0.,1.));
#3980=DIRECTION('center_axis',(0.,0.,1.));
#3981=DIRECTION('ref_axis',(1.,0.,0.));
#3982=DIRECTION('axis',(0.,0.,1.));
#3983=DIRECTION('refdir',(1.,0.,0.));
#3984=DIRECTION('center_axis',(0.,-1.,0.));
#3985=DIRECTION('ref_axis',(1.,0.,0.));
#3986=DIRECTION('center_axis',(0.,-1.,0.));
#3987=DIRECTION('ref_axis',(1.,0.,0.));
#3988=DIRECTION('center_axis',(0.,-1.,0.));
#3989=DIRECTION('ref_axis',(1.,0.,0.));
#3990=DIRECTION('',(0.,-1.,0.));
#3991=DIRECTION('center_axis',(0.,1.,0.));
#3992=DIRECTION('ref_axis',(1.,0.,0.));
#3993=DIRECTION('',(0.,0.,1.));
#3994=DIRECTION('center_axis',(0.,-1.,0.));
#3995=DIRECTION('ref_axis',(1.,0.,0.));
#3996=DIRECTION('',(0.,0.,-1.));
#3997=DIRECTION('center_axis',(0.,1.,0.));
#3998=DIRECTION('ref_axis',(1.,0.,0.));
#3999=DIRECTION('',(0.,0.,-1.));
#4000=DIRECTION('',(-1.,0.,0.));
#4001=DIRECTION('',(0.,0.,1.));
#4002=DIRECTION('center_axis',(0.,-1.,0.));
#4003=DIRECTION('ref_axis',(1.,0.,0.));
#4004=DIRECTION('',(0.,-1.,0.));
#4005=DIRECTION('',(0.,-1.,0.));
#4006=DIRECTION('center_axis',(1.,0.,0.));
#4007=DIRECTION('ref_axis',(0.,0.,1.));
#4008=DIRECTION('',(0.,0.,1.));
#4009=DIRECTION('',(0.,-1.,0.));
#4010=DIRECTION('center_axis',(-1.,0.,0.));
#4011=DIRECTION('ref_axis',(0.,0.,-1.));
#4012=DIRECTION('',(0.,0.,-1.));
#4013=DIRECTION('',(0.,1.,0.));
#4014=DIRECTION('center_axis',(0.,0.,1.));
#4015=DIRECTION('ref_axis',(1.,0.,0.));
#4016=DIRECTION('center_axis',(0.,0.,-1.));
#4017=DIRECTION('ref_axis',(1.,0.,0.));
#4018=DIRECTION('',(0.,0.,1.));
#4019=DIRECTION('center_axis',(0.,0.,-1.));
#4020=DIRECTION('ref_axis',(-1.,0.,0.));
#4021=DIRECTION('center_axis',(0.,0.,-1.));
#4022=DIRECTION('ref_axis',(-1.,0.,0.));
#4023=DIRECTION('center_axis',(0.,0.,-1.));
#4024=DIRECTION('ref_axis',(1.,0.,0.));
#4025=DIRECTION('',(0.,0.,-1.));
#4026=DIRECTION('center_axis',(0.,0.,-1.));
#4027=DIRECTION('ref_axis',(1.,0.,0.));
#4028=DIRECTION('',(0.,0.,-1.));
#4029=DIRECTION('center_axis',(0.,0.,1.));
#4030=DIRECTION('ref_axis',(1.,0.,0.));
#4031=DIRECTION('center_axis',(0.,0.,-1.));
#4032=DIRECTION('ref_axis',(-0.866025403784439,0.5,0.));
#4033=DIRECTION('',(0.,0.,-1.));
#4034=DIRECTION('center_axis',(0.,0.,1.));
#4035=DIRECTION('ref_axis',(1.,0.,0.));
#4036=DIRECTION('',(0.,0.,-1.));
#4037=DIRECTION('center_axis',(0.,0.,-1.));
#4038=DIRECTION('ref_axis',(1.,0.,0.));
#4039=DIRECTION('center_axis',(0.,0.,-1.));
#4040=DIRECTION('ref_axis',(1.,0.,0.));
#4041=DIRECTION('',(0.,0.,-1.));
#4042=DIRECTION('center_axis',(0.,0.,1.));
#4043=DIRECTION('ref_axis',(1.,0.,0.));
#4044=DIRECTION('',(0.,0.,-1.));
#4045=DIRECTION('center_axis',(0.,0.,-1.));
#4046=DIRECTION('ref_axis',(1.,0.,0.));
#4047=DIRECTION('center_axis',(0.,0.,1.));
#4048=DIRECTION('ref_axis',(1.,0.,0.));
#4049=DIRECTION('center_axis',(0.,0.,-1.));
#4050=DIRECTION('ref_axis',(1.,0.,0.));
#4051=DIRECTION('center_axis',(0.,0.,-1.));
#4052=DIRECTION('ref_axis',(1.,0.,0.));
#4053=DIRECTION('center_axis',(0.,0.,-1.));
#4054=DIRECTION('ref_axis',(1.,0.,0.));
#4055=DIRECTION('center_axis',(0.,0.,-1.));
#4056=DIRECTION('ref_axis',(1.,0.,0.));
#4057=DIRECTION('center_axis',(0.,0.,-1.));
#4058=DIRECTION('ref_axis',(1.,0.,0.));
#4059=DIRECTION('',(0.,0.,-1.));
#4060=DIRECTION('center_axis',(0.,0.,-1.));
#4061=DIRECTION('ref_axis',(1.,0.,0.));
#4062=DIRECTION('',(0.,0.,-1.));
#4063=DIRECTION('center_axis',(0.,0.,-1.));
#4064=DIRECTION('ref_axis',(1.,0.,0.));
#4065=DIRECTION('',(0.,0.,-1.));
#4066=DIRECTION('center_axis',(0.,0.,-1.));
#4067=DIRECTION('ref_axis',(1.,0.,0.));
#4068=DIRECTION('',(0.,0.,-1.));
#4069=DIRECTION('center_axis',(0.,0.,1.));
#4070=DIRECTION('ref_axis',(1.,0.,0.));
#4071=DIRECTION('',(-0.717566844774038,-0.696489643340827,0.));
#4072=DIRECTION('center_axis',(0.,0.,1.));
#4073=DIRECTION('ref_axis',(0.696489643340827,-0.717566844774038,0.));
#4074=DIRECTION('center_axis',(0.,0.,1.));
#4075=DIRECTION('ref_axis',(-0.908768955427354,-0.417299635335902,0.));
#4076=DIRECTION('center_axis',(0.,0.,1.));
#4077=DIRECTION('ref_axis',(0.908768955427354,0.417299635335902,0.));
#4078=DIRECTION('',(0.961961146992938,0.273186294817348,0.));
#4079=DIRECTION('',(-0.2443943022189,0.969675938158175,0.));
#4080=DIRECTION('center_axis',(0.,0.,1.));
#4081=DIRECTION('ref_axis',(-0.969675938158175,-0.244394302218901,0.));
#4082=DIRECTION('center_axis',(0.,0.,1.));
#4083=DIRECTION('ref_axis',(0.0929923925228028,0.995666819238687,0.));
#4084=DIRECTION('center_axis',(0.,0.,1.));
#4085=DIRECTION('ref_axis',(-0.0929923925228032,-0.995666819238687,0.));
#4086=DIRECTION('',(-0.244394302218901,-0.969675938158175,0.));
#4087=DIRECTION('',(0.961961146992938,-0.273186294817347,0.));
#4088=DIRECTION('center_axis',(0.,0.,1.));
#4089=DIRECTION('ref_axis',(0.273186294817348,0.961961146992938,0.));
#4090=DIRECTION('center_axis',(0.,0.,1.));
#4091=DIRECTION('ref_axis',(0.81577656290455,-0.578367183902786,0.));
#4092=DIRECTION('center_axis',(0.,0.,1.));
#4093=DIRECTION('ref_axis',(-0.815776562904551,0.578367183902784,0.));
#4094=DIRECTION('',(-0.717566844774037,0.696489643340828,0.));
#4095=DIRECTION('center_axis',(0.,0.,1.));
#4096=DIRECTION('ref_axis',(-1.,0.,0.));
#4097=DIRECTION('center_axis',(0.,0.,-1.));
#4098=DIRECTION('ref_axis',(-1.,0.,0.));
#4099=DIRECTION('',(0.,0.,-1.));
#4100=DIRECTION('center_axis',(0.,0.,-1.));
#4101=DIRECTION('ref_axis',(-1.,0.,0.));
#4102=DIRECTION('center_axis',(0.,0.,1.));
#4103=DIRECTION('ref_axis',(-1.,0.,0.));
#4104=DIRECTION('center_axis',(0.,0.,1.));
#4105=DIRECTION('ref_axis',(1.,0.,0.));
#4106=DIRECTION('center_axis',(0.,0.,1.));
#4107=DIRECTION('ref_axis',(1.,0.,0.));
#4108=DIRECTION('',(0.,0.,-1.));
#4109=DIRECTION('center_axis',(0.,0.,1.));
#4110=DIRECTION('ref_axis',(1.,0.,0.));
#4111=DIRECTION('center_axis',(0.,0.,-1.));
#4112=DIRECTION('ref_axis',(-0.908768955427354,-0.417299635335902,0.));
#4113=DIRECTION('',(0.,0.,-1.));
#4114=DIRECTION('center_axis',(0.,0.,1.));
#4115=DIRECTION('ref_axis',(-0.908768955427354,-0.417299635335902,0.));
#4116=DIRECTION('',(0.,0.,-1.));
#4117=DIRECTION('center_axis',(0.,0.,-1.));
#4118=DIRECTION('ref_axis',(0.908768955427354,0.417299635335902,0.));
#4119=DIRECTION('center_axis',(0.,0.,-1.));
#4120=DIRECTION('ref_axis',(0.908768955427354,0.417299635335902,0.));
#4121=DIRECTION('',(0.,0.,-1.));
#4122=DIRECTION('center_axis',(-0.273186294817348,0.961961146992938,0.));
#4123=DIRECTION('ref_axis',(0.961961146992938,0.273186294817348,0.));
#4124=DIRECTION('',(0.961961146992938,0.273186294817348,0.));
#4125=DIRECTION('',(0.,0.,-1.));
#4126=DIRECTION('',(0.,0.,-1.));
#4127=DIRECTION('center_axis',(0.696489643340827,-0.717566844774038,0.));
#4128=DIRECTION('ref_axis',(-0.717566844774038,-0.696489643340827,0.));
#4129=DIRECTION('',(-0.717566844774038,-0.696489643340827,0.));
#4130=DIRECTION('',(0.,0.,-1.));
#4131=DIRECTION('center_axis',(0.,0.,-1.));
#4132=DIRECTION('ref_axis',(0.696489643340827,-0.717566844774038,0.));
#4133=DIRECTION('center_axis',(0.,0.,-1.));
#4134=DIRECTION('ref_axis',(0.696489643340827,-0.717566844774038,0.));
#4135=DIRECTION('center_axis',(0.,0.,1.));
#4136=DIRECTION('ref_axis',(1.,0.,0.));
#4137=DIRECTION('center_axis',(0.,0.,-1.));
#4138=DIRECTION('ref_axis',(0.0929923925228028,0.995666819238687,0.));
#4139=DIRECTION('',(0.,0.,-1.));
#4140=DIRECTION('center_axis',(0.,0.,1.));
#4141=DIRECTION('ref_axis',(0.0929923925228028,0.995666819238687,0.));
#4142=DIRECTION('',(0.,0.,-1.));
#4143=DIRECTION('center_axis',(0.,0.,-1.));
#4144=DIRECTION('ref_axis',(-0.0929923925228032,-0.995666819238687,0.));
#4145=DIRECTION('center_axis',(0.,0.,-1.));
#4146=DIRECTION('ref_axis',(-0.0929923925228032,-0.995666819238687,0.));
#4147=DIRECTION('',(0.,0.,-1.));
#4148=DIRECTION('center_axis',(0.969675938158175,-0.244394302218901,0.));
#4149=DIRECTION('ref_axis',(-0.244394302218901,-0.969675938158175,0.));
#4150=DIRECTION('',(-0.244394302218901,-0.969675938158175,0.));
#4151=DIRECTION('',(0.,0.,-1.));
#4152=DIRECTION('',(0.,0.,-1.));
#4153=DIRECTION('center_axis',(-0.969675938158175,-0.2443943022189,0.));
#4154=DIRECTION('ref_axis',(-0.2443943022189,0.969675938158175,0.));
#4155=DIRECTION('',(-0.2443943022189,0.969675938158175,0.));
#4156=DIRECTION('',(0.,0.,-1.));
#4157=DIRECTION('center_axis',(0.,0.,-1.));
#4158=DIRECTION('ref_axis',(-0.969675938158175,-0.244394302218901,0.));
#4159=DIRECTION('center_axis',(0.,0.,-1.));
#4160=DIRECTION('ref_axis',(-0.969675938158175,-0.244394302218901,0.));
#4161=DIRECTION('center_axis',(0.,0.,1.));
#4162=DIRECTION('ref_axis',(1.,0.,0.));
#4163=DIRECTION('center_axis',(0.,0.,-1.));
#4164=DIRECTION('ref_axis',(0.81577656290455,-0.578367183902786,0.));
#4165=DIRECTION('',(0.,0.,-1.));
#4166=DIRECTION('center_axis',(0.,0.,1.));
#4167=DIRECTION('ref_axis',(0.81577656290455,-0.578367183902786,0.));
#4168=DIRECTION('',(0.,0.,-1.));
#4169=DIRECTION('center_axis',(0.,0.,-1.));
#4170=DIRECTION('ref_axis',(-0.815776562904551,0.578367183902784,0.));
#4171=DIRECTION('center_axis',(0.,0.,-1.));
#4172=DIRECTION('ref_axis',(-0.815776562904551,0.578367183902784,0.));
#4173=DIRECTION('',(0.,0.,-1.));
#4174=DIRECTION('center_axis',(-0.696489643340828,-0.717566844774037,0.));
#4175=DIRECTION('ref_axis',(-0.717566844774037,0.696489643340828,0.));
#4176=DIRECTION('',(-0.717566844774037,0.696489643340828,0.));
#4177=DIRECTION('',(0.,0.,-1.));
#4178=DIRECTION('',(0.,0.,-1.));
#4179=DIRECTION('center_axis',(0.,0.,-1.));
#4180=DIRECTION('ref_axis',(1.,0.,0.));
#4181=DIRECTION('center_axis',(0.,0.,-1.));
#4182=DIRECTION('ref_axis',(1.,0.,0.));
#4183=DIRECTION('',(0.,0.,-1.));
#4184=DIRECTION('',(0.,0.,-1.));
#4185=DIRECTION('center_axis',(0.273186294817347,0.961961146992938,0.));
#4186=DIRECTION('ref_axis',(0.961961146992938,-0.273186294817347,0.));
#4187=DIRECTION('',(0.961961146992938,-0.273186294817347,0.));
#4188=DIRECTION('',(0.,0.,-1.));
#4189=DIRECTION('center_axis',(0.,0.,-1.));
#4190=DIRECTION('ref_axis',(0.273186294817348,0.961961146992938,0.));
#4191=DIRECTION('center_axis',(0.,0.,-1.));
#4192=DIRECTION('ref_axis',(0.273186294817348,0.961961146992938,0.));
#4193=DIRECTION('center_axis',(0.,0.,1.));
#4194=DIRECTION('ref_axis',(1.,0.,0.));
#4195=DIRECTION('axis',(0.,0.,1.));
#4196=DIRECTION('refdir',(1.,0.,0.));
#4197=DIRECTION('center_axis',(0.,-1.,0.));
#4198=DIRECTION('ref_axis',(1.,0.,0.));
#4199=DIRECTION('center_axis',(0.,-1.,0.));
#4200=DIRECTION('ref_axis',(1.,0.,0.));
#4201=DIRECTION('center_axis',(0.,-1.,0.));
#4202=DIRECTION('ref_axis',(1.,0.,0.));
#4203=DIRECTION('',(0.,-1.,0.));
#4204=DIRECTION('center_axis',(0.,-1.,0.));
#4205=DIRECTION('ref_axis',(1.,0.,0.));
#4206=DIRECTION('',(0.,0.,-1.));
#4207=DIRECTION('',(1.,0.,0.));
#4208=DIRECTION('',(0.,0.,1.));
#4209=DIRECTION('center_axis',(0.,-1.,0.));
#4210=DIRECTION('ref_axis',(1.,0.,0.));
#4211=DIRECTION('',(0.,0.,1.));
#4212=DIRECTION('center_axis',(0.,1.,0.));
#4213=DIRECTION('ref_axis',(1.,0.,0.));
#4214=DIRECTION('',(0.,0.,-1.));
#4215=DIRECTION('center_axis',(-1.,0.,0.));
#4216=DIRECTION('ref_axis',(0.,0.,-1.));
#4217=DIRECTION('',(0.,1.,0.));
#4218=DIRECTION('',(0.,-1.,0.));
#4219=DIRECTION('',(0.,0.,1.));
#4220=DIRECTION('center_axis',(0.,1.,0.));
#4221=DIRECTION('ref_axis',(1.,0.,0.));
#4222=DIRECTION('',(0.,-1.,0.));
#4223=DIRECTION('center_axis',(1.,0.,0.));
#4224=DIRECTION('ref_axis',(0.,0.,1.));
#4225=DIRECTION('',(0.,-1.,0.));
#4226=DIRECTION('',(0.,0.,-1.));
#4227=DIRECTION('center_axis',(0.,0.,1.));
#4228=DIRECTION('ref_axis',(0.5,-0.866025403784439,0.));
#4229=DIRECTION('center_axis',(0.,0.,-1.));
#4230=DIRECTION('ref_axis',(-0.5,0.866025403784439,0.));
#4231=DIRECTION('',(0.,0.,1.));
#4232=DIRECTION('center_axis',(0.,0.,-1.));
#4233=DIRECTION('ref_axis',(0.5,-0.866025403784439,0.));
#4234=DIRECTION('center_axis',(0.,0.,-1.));
#4235=DIRECTION('ref_axis',(-0.5,0.866025403784439,0.));
#4236=DIRECTION('center_axis',(0.,0.,-1.));
#4237=DIRECTION('ref_axis',(0.5,-0.866025403784439,0.));
#4238=DIRECTION('',(0.,0.,1.));
#4239=DIRECTION('center_axis',(0.,0.,1.));
#4240=DIRECTION('ref_axis',(0.5,-0.866025403784439,0.));
#4241=DIRECTION('',(0.,0.,1.));
#4242=DIRECTION('center_axis',(0.,0.,-1.));
#4243=DIRECTION('ref_axis',(0.5,-0.866025403784439,0.));
#4244=DIRECTION('center_axis',(0.,0.,-1.));
#4245=DIRECTION('ref_axis',(0.,1.,0.));
#4246=DIRECTION('',(0.,0.,1.));
#4247=DIRECTION('center_axis',(0.,0.,-1.));
#4248=DIRECTION('ref_axis',(0.5,-0.866025403784439,0.));
#4249=DIRECTION('',(0.,0.,1.));
#4250=DIRECTION('center_axis',(0.,0.,1.));
#4251=DIRECTION('ref_axis',(0.5,-0.866025403784439,0.));
#4252=DIRECTION('center_axis',(0.,0.,-1.));
#4253=DIRECTION('ref_axis',(0.5,-0.866025403784439,0.));
#4254=DIRECTION('',(0.,0.,1.));
#4255=DIRECTION('center_axis',(0.,0.,-1.));
#4256=DIRECTION('ref_axis',(0.5,-0.866025403784439,0.));
#4257=DIRECTION('',(0.,0.,1.));
#4258=DIRECTION('center_axis',(0.,0.,1.));
#4259=DIRECTION('ref_axis',(0.5,-0.866025403784439,0.));
#4260=DIRECTION('center_axis',(0.,0.,1.));
#4261=DIRECTION('ref_axis',(0.5,-0.866025403784439,0.));
#4262=DIRECTION('center_axis',(0.,0.,-1.));
#4263=DIRECTION('ref_axis',(0.5,-0.866025403784439,0.));
#4264=DIRECTION('center_axis',(0.,0.,-1.));
#4265=DIRECTION('ref_axis',(0.5,-0.866025403784439,0.));
#4266=DIRECTION('center_axis',(0.,0.,-1.));
#4267=DIRECTION('ref_axis',(0.5,-0.866025403784439,0.));
#4268=DIRECTION('center_axis',(0.,0.,-1.));
#4269=DIRECTION('ref_axis',(0.5,-0.866025403784439,0.));
#4270=DIRECTION('center_axis',(0.,0.,-1.));
#4271=DIRECTION('ref_axis',(0.5,-0.866025403784439,0.));
#4272=DIRECTION('',(0.,0.,1.));
#4273=DIRECTION('center_axis',(0.,0.,-1.));
#4274=DIRECTION('ref_axis',(0.5,-0.866025403784439,0.));
#4275=DIRECTION('',(0.,0.,1.));
#4276=DIRECTION('center_axis',(0.,0.,-1.));
#4277=DIRECTION('ref_axis',(0.5,-0.866025403784439,0.));
#4278=DIRECTION('',(0.,0.,1.));
#4279=DIRECTION('center_axis',(0.,0.,-1.));
#4280=DIRECTION('ref_axis',(0.5,-0.866025403784439,0.));
#4281=DIRECTION('',(0.,0.,1.));
#4282=DIRECTION('center_axis',(0.,0.,1.));
#4283=DIRECTION('ref_axis',(0.5,-0.866025403784439,0.));
#4284=DIRECTION('',(0.244394302218901,0.969675938158175,0.));
#4285=DIRECTION('center_axis',(0.,0.,1.));
#4286=DIRECTION('ref_axis',(0.092992392522802,0.995666819238687,0.));
#4287=DIRECTION('center_axis',(0.,0.,1.));
#4288=DIRECTION('ref_axis',(-0.0929923925228033,-0.995666819238687,0.));
#4289=DIRECTION('center_axis',(0.,0.,1.));
#4290=DIRECTION('ref_axis',(0.969675938158175,0.244394302218901,0.));
#4291=DIRECTION('',(0.244394302218901,-0.969675938158175,0.));
#4292=DIRECTION('',(-0.961961146992938,-0.273186294817348,0.));
#4293=DIRECTION('center_axis',(0.,0.,1.));
#4294=DIRECTION('ref_axis',(-0.908768955427354,-0.417299635335902,0.));
#4295=DIRECTION('center_axis',(0.,0.,1.));
#4296=DIRECTION('ref_axis',(0.908768955427354,0.417299635335902,0.));
#4297=DIRECTION('center_axis',(0.,0.,1.));
#4298=DIRECTION('ref_axis',(-0.696489643340827,0.717566844774037,0.));
#4299=DIRECTION('',(0.717566844774038,0.696489643340827,0.));
#4300=DIRECTION('',(0.717566844774037,-0.696489643340827,0.));
#4301=DIRECTION('center_axis',(0.,0.,1.));
#4302=DIRECTION('ref_axis',(0.81577656290455,-0.578367183902785,0.));
#4303=DIRECTION('center_axis',(0.,0.,1.));
#4304=DIRECTION('ref_axis',(-0.815776562904551,0.578367183902785,0.));
#4305=DIRECTION('center_axis',(0.,0.,1.));
#4306=DIRECTION('ref_axis',(-0.273186294817348,-0.961961146992938,0.));
#4307=DIRECTION('',(-0.961961146992938,0.273186294817348,0.));
#4308=DIRECTION('center_axis',(0.,0.,1.));
#4309=DIRECTION('ref_axis',(-0.5,0.866025403784439,0.));
#4310=DIRECTION('center_axis',(0.,0.,1.));
#4311=DIRECTION('ref_axis',(-0.5,0.866025403784439,0.));
#4312=DIRECTION('',(0.,0.,-1.));
#4313=DIRECTION('center_axis',(0.,0.,1.));
#4314=DIRECTION('ref_axis',(-0.5,0.866025403784439,0.));
#4315=DIRECTION('center_axis',(0.,0.,1.));
#4316=DIRECTION('ref_axis',(-0.5,0.866025403784439,0.));
#4317=DIRECTION('center_axis',(0.,0.,1.));
#4318=DIRECTION('ref_axis',(0.5,-0.866025403784439,0.));
#4319=DIRECTION('',(0.,0.,-1.));
#4320=DIRECTION('center_axis',(0.,0.,1.));
#4321=DIRECTION('ref_axis',(0.5,-0.866025403784439,0.));
#4322=DIRECTION('center_axis',(0.,0.,1.));
#4323=DIRECTION('ref_axis',(0.5,-0.866025403784439,0.));
#4324=DIRECTION('center_axis',(0.,0.,-1.));
#4325=DIRECTION('ref_axis',(-0.815776562904551,0.578367183902785,0.));
#4326=DIRECTION('',(0.,0.,1.));
#4327=DIRECTION('center_axis',(0.,0.,1.));
#4328=DIRECTION('ref_axis',(-0.815776562904551,0.578367183902785,0.));
#4329=DIRECTION('',(0.,0.,1.));
#4330=DIRECTION('center_axis',(0.,0.,-1.));
#4331=DIRECTION('ref_axis',(0.81577656290455,-0.578367183902785,0.));
#4332=DIRECTION('',(0.,0.,1.));
#4333=DIRECTION('center_axis',(0.,0.,-1.));
#4334=DIRECTION('ref_axis',(0.81577656290455,-0.578367183902785,0.));
#4335=DIRECTION('center_axis',(-0.696489643340827,-0.717566844774037,0.));
#4336=DIRECTION('ref_axis',(0.717566844774037,-0.696489643340827,0.));
#4337=DIRECTION('',(0.,0.,1.));
#4338=DIRECTION('',(0.717566844774037,-0.696489643340827,0.));
#4339=DIRECTION('',(0.,0.,1.));
#4340=DIRECTION('center_axis',(0.273186294817348,0.961961146992938,0.));
#4341=DIRECTION('ref_axis',(-0.961961146992938,0.273186294817348,0.));
#4342=DIRECTION('',(0.,0.,1.));
#4343=DIRECTION('',(-0.961961146992938,0.273186294817348,0.));
#4344=DIRECTION('center_axis',(0.,0.,-1.));
#4345=DIRECTION('ref_axis',(-0.273186294817348,-0.961961146992938,0.));
#4346=DIRECTION('center_axis',(0.,0.,-1.));
#4347=DIRECTION('ref_axis',(-0.273186294817348,-0.961961146992938,0.));
#4348=DIRECTION('center_axis',(0.,0.,1.));
#4349=DIRECTION('ref_axis',(0.5,-0.866025403784439,0.));
#4350=DIRECTION('center_axis',(0.,0.,-1.));
#4351=DIRECTION('ref_axis',(0.908768955427354,0.417299635335902,0.));
#4352=DIRECTION('',(0.,0.,1.));
#4353=DIRECTION('center_axis',(0.,0.,1.));
#4354=DIRECTION('ref_axis',(0.908768955427354,0.417299635335902,0.));
#4355=DIRECTION('',(0.,0.,1.));
#4356=DIRECTION('center_axis',(0.,0.,-1.));
#4357=DIRECTION('ref_axis',(-0.908768955427354,-0.417299635335902,0.));
#4358=DIRECTION('',(0.,0.,1.));
#4359=DIRECTION('center_axis',(0.,0.,-1.));
#4360=DIRECTION('ref_axis',(-0.908768955427354,-0.417299635335902,0.));
#4361=DIRECTION('center_axis',(-0.273186294817348,0.961961146992938,0.));
#4362=DIRECTION('ref_axis',(-0.961961146992938,-0.273186294817348,0.));
#4363=DIRECTION('',(0.,0.,1.));
#4364=DIRECTION('',(-0.961961146992938,-0.273186294817348,0.));
#4365=DIRECTION('',(0.,0.,1.));
#4366=DIRECTION('center_axis',(0.696489643340827,-0.717566844774038,0.));
#4367=DIRECTION('ref_axis',(0.717566844774038,0.696489643340827,0.));
#4368=DIRECTION('',(0.,0.,1.));
#4369=DIRECTION('',(0.717566844774038,0.696489643340827,0.));
#4370=DIRECTION('center_axis',(0.,0.,-1.));
#4371=DIRECTION('ref_axis',(-0.696489643340827,0.717566844774037,0.));
#4372=DIRECTION('center_axis',(0.,0.,-1.));
#4373=DIRECTION('ref_axis',(-0.696489643340827,0.717566844774037,0.));
#4374=DIRECTION('center_axis',(0.,0.,1.));
#4375=DIRECTION('ref_axis',(0.5,-0.866025403784439,0.));
#4376=DIRECTION('center_axis',(0.,0.,-1.));
#4377=DIRECTION('ref_axis',(-0.0929923925228033,-0.995666819238687,0.));
#4378=DIRECTION('',(0.,0.,1.));
#4379=DIRECTION('center_axis',(0.,0.,1.));
#4380=DIRECTION('ref_axis',(-0.0929923925228033,-0.995666819238687,0.));
#4381=DIRECTION('',(0.,0.,1.));
#4382=DIRECTION('center_axis',(0.,0.,-1.));
#4383=DIRECTION('ref_axis',(0.092992392522802,0.995666819238687,0.));
#4384=DIRECTION('',(0.,0.,1.));
#4385=DIRECTION('center_axis',(0.,0.,-1.));
#4386=DIRECTION('ref_axis',(0.092992392522802,0.995666819238687,0.));
#4387=DIRECTION('center_axis',(0.969675938158175,-0.244394302218901,0.));
#4388=DIRECTION('ref_axis',(0.244394302218901,0.969675938158175,0.));
#4389=DIRECTION('',(0.,0.,1.));
#4390=DIRECTION('',(0.244394302218901,0.969675938158175,0.));
#4391=DIRECTION('',(0.,0.,1.));
#4392=DIRECTION('center_axis',(0.,0.,-1.));
#4393=DIRECTION('ref_axis',(0.5,-0.866025403784439,0.));
#4394=DIRECTION('',(0.,0.,1.));
#4395=DIRECTION('center_axis',(0.,0.,-1.));
#4396=DIRECTION('ref_axis',(0.5,-0.866025403784439,0.));
#4397=DIRECTION('',(0.,0.,1.));
#4398=DIRECTION('center_axis',(-0.969675938158175,-0.244394302218901,0.));
#4399=DIRECTION('ref_axis',(0.244394302218901,-0.969675938158175,0.));
#4400=DIRECTION('',(0.,0.,1.));
#4401=DIRECTION('',(0.244394302218901,-0.969675938158175,0.));
#4402=DIRECTION('center_axis',(0.,0.,-1.));
#4403=DIRECTION('ref_axis',(0.969675938158175,0.244394302218901,0.));
#4404=DIRECTION('center_axis',(0.,0.,-1.));
#4405=DIRECTION('ref_axis',(0.969675938158175,0.244394302218901,0.));
#4406=DIRECTION('center_axis',(0.,0.,1.));
#4407=DIRECTION('ref_axis',(0.5,-0.866025403784439,0.));
#4408=DIRECTION('axis',(0.,0.,1.));
#4409=DIRECTION('refdir',(1.,0.,0.));
#4410=DIRECTION('center_axis',(-0.855116261416916,0.,0.518436282932008));
#4411=DIRECTION('ref_axis',(0.518436282932008,0.,0.855116261416916));
#4412=DIRECTION('',(0.518436282932008,0.,0.855116261416916));
#4413=DIRECTION('',(0.,1.,0.));
#4414=DIRECTION('',(0.518436282932008,0.,0.855116261416916));
#4415=DIRECTION('',(0.,1.,0.));
#4416=DIRECTION('center_axis',(-0.876537121971153,0.,-0.481334264110221));
#4417=DIRECTION('ref_axis',(-0.481334264110221,0.,0.876537121971153));
#4418=DIRECTION('',(-0.481334264110221,0.,0.876537121971153));
#4419=DIRECTION('',(0.,1.,0.));
#4420=DIRECTION('',(-0.481334264110221,0.,0.876537121971153));
#4421=DIRECTION('center_axis',(-0.0214208605542369,0.,-0.999770547042228));
#4422=DIRECTION('ref_axis',(-0.999770547042228,0.,0.0214208605542369));
#4423=DIRECTION('',(-0.999770547042228,0.,0.0214208605542369));
#4424=DIRECTION('',(0.,1.,0.));
#4425=DIRECTION('',(-0.999770547042228,0.,0.0214208605542369));
#4426=DIRECTION('center_axis',(0.855116261416916,0.,-0.518436282932007));
#4427=DIRECTION('ref_axis',(-0.518436282932007,0.,-0.855116261416916));
#4428=DIRECTION('',(-0.518436282932007,0.,-0.855116261416916));
#4429=DIRECTION('',(0.,1.,0.));
#4430=DIRECTION('',(-0.518436282932007,0.,-0.855116261416916));
#4431=DIRECTION('center_axis',(0.876537121971153,0.,0.481334264110221));
#4432=DIRECTION('ref_axis',(0.481334264110221,0.,-0.876537121971153));
#4433=DIRECTION('',(0.481334264110221,0.,-0.876537121971153));
#4434=DIRECTION('',(0.,1.,0.));
#4435=DIRECTION('',(0.481334264110221,0.,-0.876537121971153));
#4436=DIRECTION('center_axis',(0.0214208605542369,0.,0.999770547042228));
#4437=DIRECTION('ref_axis',(0.999770547042228,0.,-0.0214208605542369));
#4438=DIRECTION('',(0.999770547042228,0.,-0.0214208605542369));
#4439=DIRECTION('',(0.999770547042228,0.,-0.0214208605542369));
#4440=DIRECTION('center_axis',(0.,1.,0.));
#4441=DIRECTION('ref_axis',(0.,0.,1.));
#4442=DIRECTION('center_axis',(0.,-1.,0.));
#4443=DIRECTION('ref_axis',(1.,0.,0.));
#4444=DIRECTION('center_axis',(0.,-1.,0.));
#4445=DIRECTION('ref_axis',(1.,0.,0.));
#4446=DIRECTION('',(0.,1.,0.));
#4447=DIRECTION('center_axis',(0.,-1.,0.));
#4448=DIRECTION('ref_axis',(1.,0.,0.));
#4449=DIRECTION('center_axis',(0.,-1.,0.));
#4450=DIRECTION('ref_axis',(1.,0.,0.));
#4451=DIRECTION('center_axis',(0.,-1.,0.));
#4452=DIRECTION('ref_axis',(1.,0.,0.));
#4453=DIRECTION('axis',(0.,0.,1.));
#4454=DIRECTION('refdir',(1.,0.,0.));
#4455=DIRECTION('center_axis',(0.855116261416916,0.,0.518436282932008));
#4456=DIRECTION('ref_axis',(0.518436282932008,0.,-0.855116261416916));
#4457=DIRECTION('',(0.518436282932008,0.,-0.855116261416916));
#4458=DIRECTION('',(0.,1.,0.));
#4459=DIRECTION('',(0.518436282932008,0.,-0.855116261416916));
#4460=DIRECTION('',(0.,1.,0.));
#4461=DIRECTION('center_axis',(0.876537121971153,0.,-0.481334264110221));
#4462=DIRECTION('ref_axis',(-0.481334264110221,0.,-0.876537121971153));
#4463=DIRECTION('',(-0.481334264110221,0.,-0.876537121971153));
#4464=DIRECTION('',(-0.481334264110221,0.,-0.876537121971153));
#4465=DIRECTION('',(0.,1.,0.));
#4466=DIRECTION('center_axis',(0.0214208605542369,0.,-0.999770547042228));
#4467=DIRECTION('ref_axis',(-0.999770547042228,0.,-0.0214208605542369));
#4468=DIRECTION('',(-0.999770547042228,0.,-0.0214208605542369));
#4469=DIRECTION('',(-0.999770547042228,0.,-0.0214208605542369));
#4470=DIRECTION('',(0.,1.,0.));
#4471=DIRECTION('center_axis',(-0.855116261416916,0.,-0.518436282932007));
#4472=DIRECTION('ref_axis',(-0.518436282932007,0.,0.855116261416916));
#4473=DIRECTION('',(-0.518436282932007,0.,0.855116261416916));
#4474=DIRECTION('',(-0.518436282932007,0.,0.855116261416916));
#4475=DIRECTION('',(0.,1.,0.));
#4476=DIRECTION('center_axis',(-0.876537121971153,0.,0.481334264110221));
#4477=DIRECTION('ref_axis',(0.481334264110221,0.,0.876537121971153));
#4478=DIRECTION('',(0.481334264110221,0.,0.876537121971153));
#4479=DIRECTION('',(0.481334264110221,0.,0.876537121971153));
#4480=DIRECTION('',(0.,1.,0.));
#4481=DIRECTION('center_axis',(-0.0214208605542369,0.,0.999770547042228));
#4482=DIRECTION('ref_axis',(0.999770547042228,0.,0.0214208605542369));
#4483=DIRECTION('',(0.999770547042228,0.,0.0214208605542369));
#4484=DIRECTION('',(0.999770547042228,0.,0.0214208605542369));
#4485=DIRECTION('center_axis',(0.,-1.,0.));
#4486=DIRECTION('ref_axis',(0.,0.,-1.));
#4487=DIRECTION('center_axis',(0.,1.,0.));
#4488=DIRECTION('ref_axis',(1.,0.,0.));
#4489=DIRECTION('center_axis',(0.,1.,0.));
#4490=DIRECTION('ref_axis',(1.,0.,0.));
#4491=DIRECTION('',(0.,-1.,0.));
#4492=DIRECTION('center_axis',(0.,1.,0.));
#4493=DIRECTION('ref_axis',(1.,0.,0.));
#4494=DIRECTION('center_axis',(0.,1.,0.));
#4495=DIRECTION('ref_axis',(1.,0.,0.));
#4496=DIRECTION('center_axis',(0.,1.,0.));
#4497=DIRECTION('ref_axis',(1.,0.,0.));
#4498=DIRECTION('axis',(0.,0.,1.));
#4499=DIRECTION('refdir',(1.,0.,0.));
#4500=DIRECTION('center_axis',(1.,0.,0.));
#4501=DIRECTION('ref_axis',(0.,0.,1.));
#4502=DIRECTION('',(0.,0.,-1.));
#4503=DIRECTION('',(0.,-1.,0.));
#4504=DIRECTION('',(0.,0.,1.));
#4505=DIRECTION('',(0.,-1.,0.));
#4506=DIRECTION('center_axis',(0.,-1.,0.));
#4507=DIRECTION('ref_axis',(1.,0.,0.));
#4508=DIRECTION('center_axis',(0.,-1.,0.));
#4509=DIRECTION('ref_axis',(1.,0.,0.));
#4510=DIRECTION('',(0.,-1.,0.));
#4511=DIRECTION('center_axis',(0.,1.,0.));
#4512=DIRECTION('ref_axis',(1.,0.,0.));
#4513=DIRECTION('center_axis',(0.,-1.,0.));
#4514=DIRECTION('ref_axis',(-1.,0.,0.));
#4515=DIRECTION('',(0.,0.,-1.));
#4516=DIRECTION('center_axis',(-1.,0.,0.));
#4517=DIRECTION('ref_axis',(0.,0.,-1.));
#4518=DIRECTION('',(0.,0.,1.));
#4519=DIRECTION('',(0.,-1.,0.));
#4520=DIRECTION('center_axis',(0.,-1.,0.));
#4521=DIRECTION('ref_axis',(-1.,0.,0.));
#4522=DIRECTION('center_axis',(0.,0.,1.));
#4523=DIRECTION('ref_axis',(-1.,0.,0.));
#4524=DIRECTION('center_axis',(0.,0.,-1.));
#4525=DIRECTION('ref_axis',(-1.,0.,0.));
#4526=DIRECTION('center_axis',(0.,0.,1.));
#4527=DIRECTION('ref_axis',(-1.,0.,0.));
#4528=DIRECTION('center_axis',(0.,0.,1.));
#4529=DIRECTION('ref_axis',(-1.,0.,0.));
#4530=DIRECTION('',(0.,0.,-1.));
#4531=DIRECTION('center_axis',(0.,0.,1.));
#4532=DIRECTION('ref_axis',(-1.,0.,0.));
#4533=DIRECTION('axis',(0.,0.,1.));
#4534=DIRECTION('refdir',(1.,0.,0.));
#4535=DIRECTION('center_axis',(-1.,0.,0.));
#4536=DIRECTION('ref_axis',(0.,0.,-1.));
#4537=DIRECTION('',(0.,0.,1.));
#4538=DIRECTION('',(0.,-1.,0.));
#4539=DIRECTION('',(0.,0.,-1.));
#4540=DIRECTION('',(0.,-1.,0.));
#4541=DIRECTION('center_axis',(0.,1.,0.));
#4542=DIRECTION('ref_axis',(1.,0.,0.));
#4543=DIRECTION('',(0.,-1.,0.));
#4544=DIRECTION('center_axis',(0.,1.,0.));
#4545=DIRECTION('ref_axis',(1.,0.,0.));
#4546=DIRECTION('center_axis',(0.,-1.,0.));
#4547=DIRECTION('ref_axis',(1.,0.,0.));
#4548=DIRECTION('',(0.,0.,1.));
#4549=DIRECTION('center_axis',(0.,1.,0.));
#4550=DIRECTION('ref_axis',(-1.,0.,0.));
#4551=DIRECTION('center_axis',(1.,0.,0.));
#4552=DIRECTION('ref_axis',(0.,0.,1.));
#4553=DIRECTION('',(0.,0.,-1.));
#4554=DIRECTION('',(0.,-1.,0.));
#4555=DIRECTION('center_axis',(0.,1.,0.));
#4556=DIRECTION('ref_axis',(-1.,0.,0.));
#4557=DIRECTION('center_axis',(0.,0.,1.));
#4558=DIRECTION('ref_axis',(-1.,0.,0.));
#4559=DIRECTION('center_axis',(0.,0.,-1.));
#4560=DIRECTION('ref_axis',(-1.,0.,0.));
#4561=DIRECTION('center_axis',(0.,0.,1.));
#4562=DIRECTION('ref_axis',(-1.,0.,0.));
#4563=DIRECTION('',(0.,0.,-1.));
#4564=DIRECTION('center_axis',(0.,0.,1.));
#4565=DIRECTION('ref_axis',(-1.,0.,0.));
#4566=DIRECTION('center_axis',(0.,0.,1.));
#4567=DIRECTION('ref_axis',(-1.,0.,0.));
#4568=DIRECTION('axis',(0.,0.,1.));
#4569=DIRECTION('refdir',(1.,0.,0.));
#4570=DIRECTION('center_axis',(0.,-1.,0.));
#4571=DIRECTION('ref_axis',(1.,0.,0.));
#4572=DIRECTION('center_axis',(0.,1.,0.));
#4573=DIRECTION('ref_axis',(1.,0.,0.));
#4574=DIRECTION('',(0.,0.,-1.));
#4575=DIRECTION('center_axis',(0.,1.,0.));
#4576=DIRECTION('ref_axis',(-1.,0.,0.));
#4577=DIRECTION('',(0.,0.,1.));
#4578=DIRECTION('center_axis',(1.,0.,0.));
#4579=DIRECTION('ref_axis',(0.,0.,1.));
#4580=DIRECTION('',(0.,-1.,0.));
#4581=DIRECTION('',(0.,0.,1.));
#4582=DIRECTION('',(0.,-1.,0.));
#4583=DIRECTION('center_axis',(0.,1.,0.));
#4584=DIRECTION('ref_axis',(1.,0.,0.));
#4585=DIRECTION('center_axis',(0.,1.,0.));
#4586=DIRECTION('ref_axis',(1.,0.,0.));
#4587=DIRECTION('',(0.,-1.,0.));
#4588=DIRECTION('center_axis',(0.,1.,0.));
#4589=DIRECTION('ref_axis',(-1.,0.,0.));
#4590=DIRECTION('',(0.,-1.,0.));
#4591=DIRECTION('center_axis',(0.,1.,0.));
#4592=DIRECTION('ref_axis',(-1.,0.,0.));
#4593=DIRECTION('center_axis',(-1.,0.,0.));
#4594=DIRECTION('ref_axis',(0.,0.,-1.));
#4595=DIRECTION('',(0.,0.,-1.));
#4596=DIRECTION('center_axis',(0.,-1.,0.));
#4597=DIRECTION('ref_axis',(1.,0.,0.));
#4598=DIRECTION('axis',(0.,0.,1.));
#4599=DIRECTION('refdir',(1.,0.,0.));
#4600=DIRECTION('center_axis',(0.,1.,0.));
#4601=DIRECTION('ref_axis',(1.,0.,0.));
#4602=DIRECTION('center_axis',(0.,-1.,0.));
#4603=DIRECTION('ref_axis',(1.,0.,0.));
#4604=DIRECTION('',(0.,0.,-1.));
#4605=DIRECTION('center_axis',(0.,-1.,0.));
#4606=DIRECTION('ref_axis',(-1.,0.,0.));
#4607=DIRECTION('',(0.,0.,1.));
#4608=DIRECTION('center_axis',(-1.,0.,0.));
#4609=DIRECTION('ref_axis',(0.,0.,-1.));
#4610=DIRECTION('',(0.,-1.,0.));
#4611=DIRECTION('',(0.,0.,-1.));
#4612=DIRECTION('',(0.,-1.,0.));
#4613=DIRECTION('center_axis',(0.,-1.,0.));
#4614=DIRECTION('ref_axis',(1.,0.,0.));
#4615=DIRECTION('',(0.,-1.,0.));
#4616=DIRECTION('center_axis',(0.,-1.,0.));
#4617=DIRECTION('ref_axis',(1.,0.,0.));
#4618=DIRECTION('center_axis',(0.,-1.,0.));
#4619=DIRECTION('ref_axis',(-1.,0.,0.));
#4620=DIRECTION('center_axis',(0.,-1.,0.));
#4621=DIRECTION('ref_axis',(-1.,0.,0.));
#4622=DIRECTION('',(0.,-1.,0.));
#4623=DIRECTION('center_axis',(1.,0.,0.));
#4624=DIRECTION('ref_axis',(0.,0.,1.));
#4625=DIRECTION('',(0.,0.,1.));
#4626=DIRECTION('center_axis',(0.,1.,0.));
#4627=DIRECTION('ref_axis',(1.,0.,0.));
#4628=DIRECTION('',(0.,0.,1.));
#4629=DIRECTION('',(1.,0.,0.));
#4630=DIRECTION('',(0.,0.,1.));
#4631=DIRECTION('',(1.,0.,0.));
#4632=DIRECTION('',(0.,0.,1.));
#4633=DIRECTION('',(1.,0.,0.));
#4634=DIRECTION('',(0.,0.,1.));
#4635=DIRECTION('',(1.,0.,0.));
#4636=DIRECTION('',(0.,0.,1.));
#4637=DIRECTION('',(1.,0.,0.));
#4638=DIRECTION('',(0.,0.,1.));
#4639=DIRECTION('',(1.,0.,0.));
#4640=DIRECTION('',(0.,0.,1.));
#4641=DIRECTION('',(1.,0.,0.));
#4642=DIRECTION('',(0.,0.,1.));
#4643=DIRECTION('',(1.,0.,0.));
#4644=DIRECTION('',(0.,0.,1.));
#4645=DIRECTION('',(1.,0.,0.));
#4646=CARTESIAN_POINT('',(0.,0.,0.));
#4647=CARTESIAN_POINT('',(0.,0.,0.));
#4648=CARTESIAN_POINT('Origin',(5.32620517920381,-3.77615934370129,0.));
#4649=CARTESIAN_POINT('',(4.51042861629926,-3.1977921597985,6.));
#4650=CARTESIAN_POINT('',(4.62971553586298,-4.49372618847532,6.));
#4651=CARTESIAN_POINT('Origin',(5.32620517920381,-3.77615934370129,6.));
#4652=CARTESIAN_POINT('',(4.62971553586298,-4.49372618847532,-1.));
#4653=CARTESIAN_POINT('',(4.62971553586298,-4.49372618847532,0.));
#4654=CARTESIAN_POINT('',(4.51042861629926,-3.1977921597985,-1.));
#4655=CARTESIAN_POINT('Origin',(5.32620517920381,-3.77615934370129,-1.));
#4656=CARTESIAN_POINT('',(4.51042861629926,-3.1977921597985,0.));
#4657=CARTESIAN_POINT('Origin',(6.06863042059311,-5.89037560471067,0.));
#4658=CARTESIAN_POINT('',(6.06863042059311,-5.89037560471067,6.));
#4659=CARTESIAN_POINT('',(3.03431521029655,-2.94518780235533,6.));
#4660=CARTESIAN_POINT('',(6.06863042059311,-5.89037560471067,-1.));
#4661=CARTESIAN_POINT('',(6.06863042059311,-5.89037560471067,0.));
#4662=CARTESIAN_POINT('',(3.03431521029655,-2.94518780235533,-1.));
#4663=CARTESIAN_POINT('Origin',(0.607147330781373,-6.50070866280939,0.));
#4664=CARTESIAN_POINT('',(0.514154938258571,-5.5050418435707,-1.));
#4665=CARTESIAN_POINT('',(1.57682326893955,-6.25631436059049,-1.));
#4666=CARTESIAN_POINT('Origin',(0.607147330781373,-6.50070866280939,-1.));
#4667=CARTESIAN_POINT('',(1.57682326893955,-6.25631436059049,6.));
#4668=CARTESIAN_POINT('',(1.57682326893955,-6.25631436059049,0.));
#4669=CARTESIAN_POINT('',(0.514154938258571,-5.5050418435707,6.));
#4670=CARTESIAN_POINT('Origin',(0.607147330781373,-6.50070866280939,6.));
#4671=CARTESIAN_POINT('',(0.514154938258571,-5.5050418435707,0.));
#4672=CARTESIAN_POINT('Origin',(1.34881215394611,-5.35164150269497,0.));
#4673=CARTESIAN_POINT('',(2.06689970121499,-8.20077591276801,-1.));
#4674=CARTESIAN_POINT('',(0.674406076973055,-2.67582075134748,-1.));
#4675=CARTESIAN_POINT('',(2.06689970121499,-8.20077591276801,6.));
#4676=CARTESIAN_POINT('',(2.06689970121499,-8.20077591276801,0.));
#4677=CARTESIAN_POINT('',(0.674406076973055,-2.67582075134748,6.));
#4678=CARTESIAN_POINT('Origin',(-0.607147330781383,-6.50070866280939,0.));
#4679=CARTESIAN_POINT('',(-0.51415493825858,-5.5050418435707,6.));
#4680=CARTESIAN_POINT('',(-1.57682326893956,-6.25631436059049,6.));
#4681=CARTESIAN_POINT('Origin',(-0.607147330781383,-6.50070866280939,6.));
#4682=CARTESIAN_POINT('',(-1.57682326893956,-6.25631436059049,-1.));
#4683=CARTESIAN_POINT('',(-1.57682326893956,-6.25631436059049,0.));
#4684=CARTESIAN_POINT('',(-0.51415493825858,-5.5050418435707,-1.));
#4685=CARTESIAN_POINT('Origin',(-0.607147330781383,-6.50070866280939,-1.));
#4686=CARTESIAN_POINT('',(-0.51415493825858,-5.5050418435707,0.));
#4687=CARTESIAN_POINT('Origin',(-2.06689970121501,-8.20077591276801,0.));
#4688=CARTESIAN_POINT('',(-2.06689970121501,-8.20077591276801,6.));
#4689=CARTESIAN_POINT('',(-1.0334498506075,-4.100387956384,6.));
#4690=CARTESIAN_POINT('',(-2.06689970121501,-8.20077591276801,-1.));
#4691=CARTESIAN_POINT('',(-2.06689970121501,-8.20077591276801,0.));
#4692=CARTESIAN_POINT('',(-1.0334498506075,-4.100387956384,-1.));
#4693=CARTESIAN_POINT('Origin',(-5.32620517920381,-3.77615934370128,0.));
#4694=CARTESIAN_POINT('',(-4.51042861629926,-3.1977921597985,-1.));
#4695=CARTESIAN_POINT('',(-4.62971553586298,-4.49372618847532,-1.));
#4696=CARTESIAN_POINT('Origin',(-5.32620517920381,-3.77615934370128,-1.));
#4697=CARTESIAN_POINT('',(-4.62971553586298,-4.49372618847532,6.));
#4698=CARTESIAN_POINT('',(-4.62971553586298,-4.49372618847532,0.));
#4699=CARTESIAN_POINT('',(-4.51042861629926,-3.1977921597985,6.));
#4700=CARTESIAN_POINT('Origin',(-5.32620517920381,-3.77615934370128,6.));
#4701=CARTESIAN_POINT('',(-4.51042861629926,-3.1977921597985,0.));
#4702=CARTESIAN_POINT('Origin',(-3.96025141630791,-3.84392634159802,0.));
#4703=CARTESIAN_POINT('',(-6.06863042059311,-5.89037560471066,-1.));
#4704=CARTESIAN_POINT('',(-1.98012570815396,-1.92196317079901,-1.));
#4705=CARTESIAN_POINT('',(-6.06863042059311,-5.89037560471066,6.));
#4706=CARTESIAN_POINT('',(-6.06863042059311,-5.89037560471066,0.));
#4707=CARTESIAN_POINT('',(-1.98012570815396,-1.92196317079901,6.));
#4708=CARTESIAN_POINT('Origin',(-5.93335250998519,-2.72454931910811,0.));
#4709=CARTESIAN_POINT('',(-5.02458355455784,-2.3072496837722,6.));
#4710=CARTESIAN_POINT('',(-6.20653880480254,-1.76258817211517,6.));
#4711=CARTESIAN_POINT('Origin',(-5.93335250998519,-2.72454931910811,6.));
#4712=CARTESIAN_POINT('',(-6.20653880480254,-1.76258817211517,-1.));
#4713=CARTESIAN_POINT('',(-6.20653880480254,-1.76258817211517,0.));
#4714=CARTESIAN_POINT('',(-5.02458355455784,-2.3072496837722,-1.));
#4715=CARTESIAN_POINT('Origin',(-5.93335250998519,-2.72454931910811,-1.));
#4716=CARTESIAN_POINT('',(-5.02458355455784,-2.3072496837722,0.));
#4717=CARTESIAN_POINT('Origin',(-8.13553012180811,-2.31040030805734,0.));
#4718=CARTESIAN_POINT('',(-8.13553012180811,-2.31040030805734,6.));
#4719=CARTESIAN_POINT('',(-4.06776506090406,-1.15520015402867,6.));
#4720=CARTESIAN_POINT('',(-8.13553012180811,-2.31040030805734,-1.));
#4721=CARTESIAN_POINT('',(-8.13553012180811,-2.31040030805734,0.));
#4722=CARTESIAN_POINT('',(-4.06776506090406,-1.15520015402867,-1.));
#4723=CARTESIAN_POINT('Origin',(-5.93335250998519,2.72454931910811,0.));
#4724=CARTESIAN_POINT('',(-5.02458355455784,2.3072496837722,-1.));
#4725=CARTESIAN_POINT('',(-6.20653880480254,1.76258817211517,-1.));
#4726=CARTESIAN_POINT('Origin',(-5.93335250998519,2.72454931910811,-1.));
#4727=CARTESIAN_POINT('',(-6.20653880480254,1.76258817211517,6.));
#4728=CARTESIAN_POINT('',(-6.20653880480254,1.76258817211517,0.));
#4729=CARTESIAN_POINT('',(-5.02458355455784,2.3072496837722,6.));
#4730=CARTESIAN_POINT('Origin',(-5.93335250998519,2.72454931910811,6.));
#4731=CARTESIAN_POINT('',(-5.02458355455784,2.3072496837722,0.));
#4732=CARTESIAN_POINT('Origin',(-5.30906357025402,1.50771516109694,0.));
#4733=CARTESIAN_POINT('',(-8.13553012180811,2.31040030805735,-1.));
#4734=CARTESIAN_POINT('',(-2.65453178512701,0.75385758054847,-1.));
#4735=CARTESIAN_POINT('',(-8.13553012180811,2.31040030805735,6.));
#4736=CARTESIAN_POINT('',(-8.13553012180811,2.31040030805735,0.));
#4737=CARTESIAN_POINT('',(-2.65453178512701,0.75385758054847,6.));
#4738=CARTESIAN_POINT('Origin',(-5.32620517920381,3.77615934370128,0.));
#4739=CARTESIAN_POINT('',(-4.51042861629926,3.1977921597985,6.));
#4740=CARTESIAN_POINT('',(-4.62971553586298,4.49372618847532,6.));
#4741=CARTESIAN_POINT('Origin',(-5.32620517920381,3.77615934370128,6.));
#4742=CARTESIAN_POINT('',(-4.62971553586298,4.49372618847532,-1.));
#4743=CARTESIAN_POINT('',(-4.62971553586298,4.49372618847532,0.));
#4744=CARTESIAN_POINT('',(-4.51042861629926,3.1977921597985,-1.));
#4745=CARTESIAN_POINT('Origin',(-5.32620517920381,3.77615934370128,-1.));
#4746=CARTESIAN_POINT('',(-4.51042861629926,3.1977921597985,0.));
#4747=CARTESIAN_POINT('Origin',(-6.06863042059311,5.89037560471066,0.));
#4748=CARTESIAN_POINT('',(-6.06863042059311,5.89037560471066,6.));
#4749=CARTESIAN_POINT('',(-3.03431521029656,2.94518780235533,6.));
#4750=CARTESIAN_POINT('',(-6.06863042059311,5.89037560471066,-1.));
#4751=CARTESIAN_POINT('',(-6.06863042059311,5.89037560471066,0.));
#4752=CARTESIAN_POINT('',(-3.03431521029656,2.94518780235533,-1.));
#4753=CARTESIAN_POINT('Origin',(-0.607147330781379,6.50070866280939,0.));
#4754=CARTESIAN_POINT('',(-0.514154938258576,5.5050418435707,-1.));
#4755=CARTESIAN_POINT('',(-1.57682326893955,6.25631436059049,-1.));
#4756=CARTESIAN_POINT('Origin',(-0.607147330781379,6.50070866280939,-1.));
#4757=CARTESIAN_POINT('',(-1.57682326893955,6.25631436059049,6.));
#4758=CARTESIAN_POINT('',(-1.57682326893955,6.25631436059049,0.));
#4759=CARTESIAN_POINT('',(-0.514154938258576,5.5050418435707,6.));
#4760=CARTESIAN_POINT('Origin',(-0.607147330781379,6.50070866280939,6.));
#4761=CARTESIAN_POINT('',(-0.514154938258576,5.5050418435707,0.));
#4762=CARTESIAN_POINT('Origin',(-1.34881215394611,5.35164150269497,0.));
#4763=CARTESIAN_POINT('',(-2.066899701215,8.20077591276801,-1.));
#4764=CARTESIAN_POINT('',(-0.674406076973057,2.67582075134748,-1.));
#4765=CARTESIAN_POINT('',(-2.066899701215,8.20077591276801,6.));
#4766=CARTESIAN_POINT('',(-2.066899701215,8.20077591276801,0.));
#4767=CARTESIAN_POINT('',(-0.674406076973057,2.67582075134748,6.));
#4768=CARTESIAN_POINT('Origin',(0.60714733078138,6.50070866280939,0.));
#4769=CARTESIAN_POINT('',(0.514154938258577,5.5050418435707,6.));
#4770=CARTESIAN_POINT('',(1.57682326893956,6.25631436059049,6.));
#4771=CARTESIAN_POINT('Origin',(0.60714733078138,6.50070866280939,6.));
#4772=CARTESIAN_POINT('',(1.57682326893956,6.25631436059049,-1.));
#4773=CARTESIAN_POINT('',(1.57682326893956,6.25631436059049,0.));
#4774=CARTESIAN_POINT('',(0.514154938258577,5.5050418435707,-1.));
#4775=CARTESIAN_POINT('Origin',(0.60714733078138,6.50070866280939,-1.));
#4776=CARTESIAN_POINT('',(0.514154938258577,5.5050418435707,0.));
#4777=CARTESIAN_POINT('Origin',(2.066899701215,8.20077591276801,0.));
#4778=CARTESIAN_POINT('',(2.066899701215,8.20077591276801,6.));
#4779=CARTESIAN_POINT('',(1.0334498506075,4.100387956384,6.));
#4780=CARTESIAN_POINT('',(2.066899701215,8.20077591276801,-1.));
#4781=CARTESIAN_POINT('',(2.066899701215,8.20077591276801,0.));
#4782=CARTESIAN_POINT('',(1.0334498506075,4.100387956384,-1.));
#4783=CARTESIAN_POINT('Origin',(5.32620517920381,3.77615934370128,0.));
#4784=CARTESIAN_POINT('',(4.51042861629926,3.1977921597985,-1.));
#4785=CARTESIAN_POINT('',(4.62971553586298,4.49372618847532,-1.));
#4786=CARTESIAN_POINT('Origin',(5.32620517920381,3.77615934370128,-1.));
#4787=CARTESIAN_POINT('',(4.62971553586298,4.49372618847532,6.));
#4788=CARTESIAN_POINT('',(4.62971553586298,4.49372618847532,0.));
#4789=CARTESIAN_POINT('',(4.51042861629926,3.1977921597985,6.));
#4790=CARTESIAN_POINT('Origin',(5.32620517920381,3.77615934370128,6.));
#4791=CARTESIAN_POINT('',(4.51042861629926,3.1977921597985,0.));
#4792=CARTESIAN_POINT('Origin',(3.96025141630791,3.84392634159803,0.));
#4793=CARTESIAN_POINT('',(6.06863042059311,5.89037560471066,-1.));
#4794=CARTESIAN_POINT('',(1.98012570815396,1.92196317079901,-1.));
#4795=CARTESIAN_POINT('',(6.06863042059311,5.89037560471066,6.));
#4796=CARTESIAN_POINT('',(6.06863042059311,5.89037560471066,0.));
#4797=CARTESIAN_POINT('',(1.98012570815396,1.92196317079901,6.));
#4798=CARTESIAN_POINT('Ctrl Pts',(6.60014603862877,-10.0218796774244,-3.75));
#4799=CARTESIAN_POINT('Ctrl Pts',(6.60014603862877,-10.0218796774244,12.75));
#4800=CARTESIAN_POINT('Ctrl Pts',(6.60293150665658,-10.0085665785717,-3.75));
#4801=CARTESIAN_POINT('Ctrl Pts',(6.60293150665658,-10.0085665785717,12.75));
#4802=CARTESIAN_POINT('Ctrl Pts',(6.60844558393655,-9.98194823089969,-3.75));
#4803=CARTESIAN_POINT('Ctrl Pts',(6.60844558393655,-9.98194823089969,12.75));
#4804=CARTESIAN_POINT('Ctrl Pts',(6.61654612354182,-9.94204425953052,-3.75));
#4805=CARTESIAN_POINT('Ctrl Pts',(6.61654612354182,-9.94204425953052,12.75));
#4806=CARTESIAN_POINT('Ctrl Pts',(6.62700557693595,-9.88888607996273,-3.75));
#4807=CARTESIAN_POINT('Ctrl Pts',(6.62700557693595,-9.88888607996273,12.75));
#4808=CARTESIAN_POINT('Ctrl Pts',(6.63951038900666,-9.82251725114899,-3.75));
#4809=CARTESIAN_POINT('Ctrl Pts',(6.63951038900666,-9.82251725114899,12.75));
#4810=CARTESIAN_POINT('Ctrl Pts',(6.65144464725858,-9.75622826411014,-3.75));
#4811=CARTESIAN_POINT('Ctrl Pts',(6.65144464725858,-9.75622826411014,12.75));
#4812=CARTESIAN_POINT('Ctrl Pts',(6.66280711160719,-9.69002090483258,-3.75));
#4813=CARTESIAN_POINT('Ctrl Pts',(6.66280711160719,-9.69002090483258,12.75));
#4814=CARTESIAN_POINT('Ctrl Pts',(6.6735964736696,-9.62389802250188,-3.75));
#4815=CARTESIAN_POINT('Ctrl Pts',(6.6735964736696,-9.62389802250188,12.75));
#4816=CARTESIAN_POINT('Ctrl Pts',(6.68381150859182,-9.55786385494287,-3.75));
#4817=CARTESIAN_POINT('Ctrl Pts',(6.68381150859182,-9.55786385494287,12.75));
#4818=CARTESIAN_POINT('Ctrl Pts',(6.69345108162376,-9.49192378686254,-3.75));
#4819=CARTESIAN_POINT('Ctrl Pts',(6.69345108162376,-9.49192378686254,12.75));
#4820=CARTESIAN_POINT('Ctrl Pts',(6.70251410760818,-9.42608392519667,-3.75));
#4821=CARTESIAN_POINT('Ctrl Pts',(6.70251410760818,-9.42608392519667,12.75));
#4822=CARTESIAN_POINT('Ctrl Pts',(6.71099953007123,-9.36035072031877,-3.75));
#4823=CARTESIAN_POINT('Ctrl Pts',(6.71099953007123,-9.36035072031877,12.75));
#4824=CARTESIAN_POINT('Ctrl Pts',(6.71890629646186,-9.29473060155551,-3.75));
#4825=CARTESIAN_POINT('Ctrl Pts',(6.71890629646186,-9.29473060155551,12.75));
#4826=CARTESIAN_POINT('Ctrl Pts',(6.72623333926845,-9.22922952332026,-3.75));
#4827=CARTESIAN_POINT('Ctrl Pts',(6.72623333926845,-9.22922952332026,12.75));
#4828=CARTESIAN_POINT('Ctrl Pts',(6.73297955932547,-9.16385288053588,-3.75));
#4829=CARTESIAN_POINT('Ctrl Pts',(6.73297955932547,-9.16385288053588,12.75));
#4830=CARTESIAN_POINT('Ctrl Pts',(6.73914381348522,-9.09860577342166,-3.75));
#4831=CARTESIAN_POINT('Ctrl Pts',(6.73914381348522,-9.09860577342166,12.75));
#4832=CARTESIAN_POINT('Ctrl Pts',(6.74472490424422,-9.03349318036199,-3.75));
#4833=CARTESIAN_POINT('Ctrl Pts',(6.74472490424422,-9.03349318036199,12.75));
#4834=CARTESIAN_POINT('Ctrl Pts',(6.74972157399228,-8.96852015431047,-3.75));
#4835=CARTESIAN_POINT('Ctrl Pts',(6.74972157399228,-8.96852015431047,12.75));
#4836=CARTESIAN_POINT('Ctrl Pts',(6.75413249860575,-8.90369203916218,-3.75));
#4837=CARTESIAN_POINT('Ctrl Pts',(6.75413249860575,-8.90369203916218,12.75));
#4838=CARTESIAN_POINT('Ctrl Pts',(6.75795629519249,-8.83901457377472,-3.75));
#4839=CARTESIAN_POINT('Ctrl Pts',(6.75795629519249,-8.83901457377472,12.75));
#4840=CARTESIAN_POINT('Ctrl Pts',(6.76119155448274,-8.77449374557665,-3.75));
#4841=CARTESIAN_POINT('Ctrl Pts',(6.76119155448274,-8.77449374557665,12.75));
#4842=CARTESIAN_POINT('Ctrl Pts',(6.76383687353852,-8.710135693856,-3.75));
#4843=CARTESIAN_POINT('Ctrl Pts',(6.76383687353852,-8.710135693856,12.75));
#4844=CARTESIAN_POINT('Ctrl Pts',(6.76589088878265,-8.64594659806299,-3.75));
#4845=CARTESIAN_POINT('Ctrl Pts',(6.76589088878265,-8.64594659806299,12.75));
#4846=CARTESIAN_POINT('Ctrl Pts',(6.76735232235634,-8.5819325577994,-3.75));
#4847=CARTESIAN_POINT('Ctrl Pts',(6.76735232235634,-8.5819325577994,12.75));
#4848=CARTESIAN_POINT('Ctrl Pts',(6.76822000004554,-8.51809951610774,-3.75));
#4849=CARTESIAN_POINT('Ctrl Pts',(6.76822000004554,-8.51809951610774,12.75));
#4850=CARTESIAN_POINT('Ctrl Pts',(6.76849272647565,-8.45445340444927,-3.75));
#4851=CARTESIAN_POINT('Ctrl Pts',(6.76849272647565,-8.45445340444927,12.75));
#4852=CARTESIAN_POINT('Ctrl Pts',(6.76816918165127,-8.39100025749019,-3.75));
#4853=CARTESIAN_POINT('Ctrl Pts',(6.76816918165127,-8.39100025749019,12.75));
#4854=CARTESIAN_POINT('Ctrl Pts',(6.76724781676281,-8.32774633509908,-3.75));
#4855=CARTESIAN_POINT('Ctrl Pts',(6.76724781676281,-8.32774633509908,12.75));
#4856=CARTESIAN_POINT('Ctrl Pts',(6.76572674650934,-8.26469824786603,-3.75));
#4857=CARTESIAN_POINT('Ctrl Pts',(6.76572674650934,-8.26469824786603,12.75));
#4858=CARTESIAN_POINT('Ctrl Pts',(6.76360366961639,-8.20186305794855,-3.75));
#4859=CARTESIAN_POINT('Ctrl Pts',(6.76360366961639,-8.20186305794855,12.75));
#4860=CARTESIAN_POINT('Ctrl Pts',(6.76087611417305,-8.13924806419108,-3.75));
#4861=CARTESIAN_POINT('Ctrl Pts',(6.76087611417305,-8.13924806419108,12.75));
#4862=CARTESIAN_POINT('Ctrl Pts',(6.75754166486089,-8.07686060726828,-3.75));
#4863=CARTESIAN_POINT('Ctrl Pts',(6.75754166486089,-8.07686060726828,12.75));
#4864=CARTESIAN_POINT('Ctrl Pts',(6.75359819949754,-8.01470786732019,-3.75));
#4865=CARTESIAN_POINT('Ctrl Pts',(6.75359819949754,-8.01470786732019,12.75));
#4866=CARTESIAN_POINT('Ctrl Pts',(6.7490441308376,-7.95279665937614,-3.75));
#4867=CARTESIAN_POINT('Ctrl Pts',(6.7490441308376,-7.95279665937614,12.75));
#4868=CARTESIAN_POINT('Ctrl Pts',(6.74387863902607,-7.89113323756913,-3.75));
#4869=CARTESIAN_POINT('Ctrl Pts',(6.74387863902607,-7.89113323756913,12.75));
#4870=CARTESIAN_POINT('Ctrl Pts',(6.73810106562748,-7.82972378407325,-3.75));
#4871=CARTESIAN_POINT('Ctrl Pts',(6.73810106562748,-7.82972378407325,12.75));
#4872=CARTESIAN_POINT('Ctrl Pts',(6.73171032576035,-7.76857488460784,-3.75));
#4873=CARTESIAN_POINT('Ctrl Pts',(6.73171032576035,-7.76857488460784,12.75));
#4874=CARTESIAN_POINT('Ctrl Pts',(6.72470431659336,-7.70769400824503,-3.75));
#4875=CARTESIAN_POINT('Ctrl Pts',(6.72470431659336,-7.70769400824503,12.75));
#4876=CARTESIAN_POINT('Ctrl Pts',(6.71707933277187,-7.6470899828899,-3.75));
#4877=CARTESIAN_POINT('Ctrl Pts',(6.71707933277187,-7.6470899828899,12.75));
#4878=CARTESIAN_POINT('Ctrl Pts',(6.70882947565317,-7.58677347699226,-3.75));
#4879=CARTESIAN_POINT('Ctrl Pts',(6.70882947565317,-7.58677347699226,12.75));
#4880=CARTESIAN_POINT('Ctrl Pts',(6.69994799095523,-7.52675593674633,-3.75));
#4881=CARTESIAN_POINT('Ctrl Pts',(6.69994799095523,-7.52675593674633,12.75));
#4882=CARTESIAN_POINT('Ctrl Pts',(6.69042862091103,-7.46704851290035,-3.75));
#4883=CARTESIAN_POINT('Ctrl Pts',(6.69042862091103,-7.46704851290035,12.75));
#4884=CARTESIAN_POINT('Ctrl Pts',(6.68026694677667,-7.40766099640558,-3.75));
#4885=CARTESIAN_POINT('Ctrl Pts',(6.68026694677667,-7.40766099640558,12.75));
#4886=CARTESIAN_POINT('Ctrl Pts',(6.66946176275797,-7.34860073021492,-3.75));
#4887=CARTESIAN_POINT('Ctrl Pts',(6.66946176275797,-7.34860073021492,12.75));
#4888=CARTESIAN_POINT('Ctrl Pts',(6.65801638970246,-7.28987157005224,-3.75));
#4889=CARTESIAN_POINT('Ctrl Pts',(6.65801638970246,-7.28987157005224,12.75));
#4890=CARTESIAN_POINT('Ctrl Pts',(6.64593535561052,-7.23147652896403,-3.75));
#4891=CARTESIAN_POINT('Ctrl Pts',(6.64593535561052,-7.23147652896403,12.75));
#4892=CARTESIAN_POINT('Ctrl Pts',(6.63322107969568,-7.17342042004756,-3.75));
#4893=CARTESIAN_POINT('Ctrl Pts',(6.63322107969568,-7.17342042004756,12.75));
#4894=CARTESIAN_POINT('Ctrl Pts',(6.6198706660591,-7.1157124131703,-3.75));
#4895=CARTESIAN_POINT('Ctrl Pts',(6.6198706660591,-7.1157124131703,12.75));
#4896=CARTESIAN_POINT('Ctrl Pts',(6.60587239994885,-7.05836882883084,-3.75));
#4897=CARTESIAN_POINT('Ctrl Pts',(6.60587239994885,-7.05836882883084,12.75));
#4898=CARTESIAN_POINT('Ctrl Pts',(6.5912030640433,-7.00141528186887,-3.75));
#4899=CARTESIAN_POINT('Ctrl Pts',(6.5912030640433,-7.00141528186887,12.75));
#4900=CARTESIAN_POINT('Ctrl Pts',(6.5758359541656,-6.94488033148854,-3.75));
#4901=CARTESIAN_POINT('Ctrl Pts',(6.5758359541656,-6.94488033148854,12.75));
#4902=CARTESIAN_POINT('Ctrl Pts',(6.55974857229919,-6.88878938806038,-3.75));
#4903=CARTESIAN_POINT('Ctrl Pts',(6.55974857229919,-6.88878938806038,12.75));
#4904=CARTESIAN_POINT('Ctrl Pts',(6.54292981913303,-6.83315901897032,-3.75));
#4905=CARTESIAN_POINT('Ctrl Pts',(6.54292981913303,-6.83315901897032,12.75));
#4906=CARTESIAN_POINT('Ctrl Pts',(6.52538888693355,-6.77798990345397,-3.75));
#4907=CARTESIAN_POINT('Ctrl Pts',(6.52538888693355,-6.77798990345397,12.75));
#4908=CARTESIAN_POINT('Ctrl Pts',(6.50715912032692,-6.72326378902152,-3.75));
#4909=CARTESIAN_POINT('Ctrl Pts',(6.50715912032692,-6.72326378902152,12.75));
#4910=CARTESIAN_POINT('Ctrl Pts',(6.48827758470622,-6.66895976394945,-3.75));
#4911=CARTESIAN_POINT('Ctrl Pts',(6.48827758470622,-6.66895976394945,12.75));
#4912=CARTESIAN_POINT('Ctrl Pts',(6.46876645798848,-6.61506907935741,-3.75));
#4913=CARTESIAN_POINT('Ctrl Pts',(6.46876645798848,-6.61506907935741,12.75));
#4914=CARTESIAN_POINT('Ctrl Pts',(6.44861636238489,-6.56160843323029,-3.75));
#4915=CARTESIAN_POINT('Ctrl Pts',(6.44861636238489,-6.56160843323029,12.75));
#4916=CARTESIAN_POINT('Ctrl Pts',(6.42776254872513,-6.50863892931077,-3.75));
#4917=CARTESIAN_POINT('Ctrl Pts',(6.42776254872513,-6.50863892931077,12.75));
#4918=CARTESIAN_POINT('Ctrl Pts',(6.40608444337877,-6.45626649182453,-3.75));
#4919=CARTESIAN_POINT('Ctrl Pts',(6.40608444337877,-6.45626649182453,12.75));
#4920=CARTESIAN_POINT('Ctrl Pts',(6.38345478017075,-6.404602962683,-3.75));
#4921=CARTESIAN_POINT('Ctrl Pts',(6.38345478017075,-6.404602962683,12.75));
#4922=CARTESIAN_POINT('Ctrl Pts',(6.35978286360965,-6.35373180396277,-3.75));
#4923=CARTESIAN_POINT('Ctrl Pts',(6.35978286360965,-6.35373180396277,12.75));
#4924=CARTESIAN_POINT('Ctrl Pts',(6.33505137069502,-6.30367904881887,-3.75));
#4925=CARTESIAN_POINT('Ctrl Pts',(6.33505137069502,-6.30367904881887,12.75));
#4926=CARTESIAN_POINT('Ctrl Pts',(6.309377504208,-6.25436463761971,-3.75));
#4927=CARTESIAN_POINT('Ctrl Pts',(6.309377504208,-6.25436463761971,12.75));
#4928=CARTESIAN_POINT('Ctrl Pts',(6.28297985424307,-6.20562962932065,-3.75));
#4929=CARTESIAN_POINT('Ctrl Pts',(6.28297985424307,-6.20562962932065,12.75));
#4930=CARTESIAN_POINT('Ctrl Pts',(6.25605474467853,-6.15733614814836,-3.75));
#4931=CARTESIAN_POINT('Ctrl Pts',(6.25605474467853,-6.15733614814836,12.75));
#4932=CARTESIAN_POINT('Ctrl Pts',(6.22866991793491,-6.10945353793714,-3.75));
#4933=CARTESIAN_POINT('Ctrl Pts',(6.22866991793491,-6.10945353793714,12.75));
#4934=CARTESIAN_POINT('Ctrl Pts',(6.20066685685754,-6.06213722636287,-3.75));
#4935=CARTESIAN_POINT('Ctrl Pts',(6.20066685685754,-6.06213722636287,12.75));
#4936=CARTESIAN_POINT('Ctrl Pts',(6.17151878498998,-6.01584411654484,-3.75));
#4937=CARTESIAN_POINT('Ctrl Pts',(6.17151878498998,-6.01584411654484,12.75));
#4938=CARTESIAN_POINT('Ctrl Pts',(6.14045331140033,-5.97123031969247,-3.75));
#4939=CARTESIAN_POINT('Ctrl Pts',(6.14045331140033,-5.97123031969247,12.75));
#4940=CARTESIAN_POINT('Ctrl Pts',(6.11342775487885,-5.9374218385168,-3.75));
#4941=CARTESIAN_POINT('Ctrl Pts',(6.11342775487885,-5.9374218385168,12.75));
#4942=CARTESIAN_POINT('Ctrl Pts',(6.09164867072823,-5.91336588048664,-3.75));
#4943=CARTESIAN_POINT('Ctrl Pts',(6.09164867072823,-5.91336588048664,12.75));
#4944=CARTESIAN_POINT('Ctrl Pts',(6.07642118935899,-5.89793753402585,-3.75));
#4945=CARTESIAN_POINT('Ctrl Pts',(6.07642118935899,-5.89793753402585,12.75));
#4946=CARTESIAN_POINT('Ctrl Pts',(6.06863042059311,-5.89037560471067,-3.75));
#4947=CARTESIAN_POINT('Ctrl Pts',(6.06863042059311,-5.89037560471067,12.75));
#4948=CARTESIAN_POINT('',(6.60014603862874,-10.0218796774245,-1.));
#4949=CARTESIAN_POINT('Ctrl Pts',(6.60014603862877,-10.0218796774244,-1.));
#4950=CARTESIAN_POINT('Ctrl Pts',(6.60293150665658,-10.0085665785717,-1.));
#4951=CARTESIAN_POINT('Ctrl Pts',(6.60844558393655,-9.98194823089969,-1.));
#4952=CARTESIAN_POINT('Ctrl Pts',(6.61654612354182,-9.94204425953052,-1.));
#4953=CARTESIAN_POINT('Ctrl Pts',(6.62700557693595,-9.88888607996273,-1.));
#4954=CARTESIAN_POINT('Ctrl Pts',(6.63951038900666,-9.82251725114899,-1.));
#4955=CARTESIAN_POINT('Ctrl Pts',(6.65144464725858,-9.75622826411014,-1.));
#4956=CARTESIAN_POINT('Ctrl Pts',(6.66280711160719,-9.69002090483258,-1.));
#4957=CARTESIAN_POINT('Ctrl Pts',(6.6735964736696,-9.62389802250188,-1.));
#4958=CARTESIAN_POINT('Ctrl Pts',(6.68381150859182,-9.55786385494287,-1.));
#4959=CARTESIAN_POINT('Ctrl Pts',(6.69345108162376,-9.49192378686254,-1.));
#4960=CARTESIAN_POINT('Ctrl Pts',(6.70251410760818,-9.42608392519667,-1.));
#4961=CARTESIAN_POINT('Ctrl Pts',(6.71099953007123,-9.36035072031877,-1.));
#4962=CARTESIAN_POINT('Ctrl Pts',(6.71890629646186,-9.29473060155551,-1.));
#4963=CARTESIAN_POINT('Ctrl Pts',(6.72623333926845,-9.22922952332026,-1.));
#4964=CARTESIAN_POINT('Ctrl Pts',(6.73297955932547,-9.16385288053588,-1.));
#4965=CARTESIAN_POINT('Ctrl Pts',(6.73914381348522,-9.09860577342166,-1.));
#4966=CARTESIAN_POINT('Ctrl Pts',(6.74472490424422,-9.03349318036199,-1.));
#4967=CARTESIAN_POINT('Ctrl Pts',(6.74972157399228,-8.96852015431047,-1.));
#4968=CARTESIAN_POINT('Ctrl Pts',(6.75413249860575,-8.90369203916218,-1.));
#4969=CARTESIAN_POINT('Ctrl Pts',(6.75795629519249,-8.83901457377472,-1.));
#4970=CARTESIAN_POINT('Ctrl Pts',(6.76119155448274,-8.77449374557665,-1.));
#4971=CARTESIAN_POINT('Ctrl Pts',(6.76383687353852,-8.710135693856,-1.));
#4972=CARTESIAN_POINT('Ctrl Pts',(6.76589088878265,-8.64594659806299,-1.));
#4973=CARTESIAN_POINT('Ctrl Pts',(6.76735232235634,-8.5819325577994,-1.));
#4974=CARTESIAN_POINT('Ctrl Pts',(6.76822000004554,-8.51809951610774,-1.));
#4975=CARTESIAN_POINT('Ctrl Pts',(6.76849272647565,-8.45445340444927,-1.));
#4976=CARTESIAN_POINT('Ctrl Pts',(6.76816918165127,-8.39100025749019,-1.));
#4977=CARTESIAN_POINT('Ctrl Pts',(6.76724781676281,-8.32774633509908,-1.));
#4978=CARTESIAN_POINT('Ctrl Pts',(6.76572674650934,-8.26469824786603,-1.));
#4979=CARTESIAN_POINT('Ctrl Pts',(6.76360366961639,-8.20186305794855,-1.));
#4980=CARTESIAN_POINT('Ctrl Pts',(6.76087611417305,-8.13924806419108,-1.));
#4981=CARTESIAN_POINT('Ctrl Pts',(6.75754166486089,-8.07686060726828,-1.));
#4982=CARTESIAN_POINT('Ctrl Pts',(6.75359819949754,-8.01470786732019,-1.));
#4983=CARTESIAN_POINT('Ctrl Pts',(6.7490441308376,-7.95279665937614,-1.));
#4984=CARTESIAN_POINT('Ctrl Pts',(6.74387863902607,-7.89113323756913,-1.));
#4985=CARTESIAN_POINT('Ctrl Pts',(6.73810106562748,-7.82972378407325,-1.));
#4986=CARTESIAN_POINT('Ctrl Pts',(6.73171032576035,-7.76857488460784,-1.));
#4987=CARTESIAN_POINT('Ctrl Pts',(6.72470431659336,-7.70769400824503,-1.));
#4988=CARTESIAN_POINT('Ctrl Pts',(6.71707933277187,-7.6470899828899,-1.));
#4989=CARTESIAN_POINT('Ctrl Pts',(6.70882947565317,-7.58677347699226,-1.));
#4990=CARTESIAN_POINT('Ctrl Pts',(6.69994799095523,-7.52675593674633,-1.));
#4991=CARTESIAN_POINT('Ctrl Pts',(6.69042862091103,-7.46704851290035,-1.));
#4992=CARTESIAN_POINT('Ctrl Pts',(6.68026694677667,-7.40766099640558,-1.));
#4993=CARTESIAN_POINT('Ctrl Pts',(6.66946176275797,-7.34860073021492,-1.));
#4994=CARTESIAN_POINT('Ctrl Pts',(6.65801638970246,-7.28987157005224,-1.));
#4995=CARTESIAN_POINT('Ctrl Pts',(6.64593535561052,-7.23147652896403,-1.));
#4996=CARTESIAN_POINT('Ctrl Pts',(6.63322107969568,-7.17342042004756,-1.));
#4997=CARTESIAN_POINT('Ctrl Pts',(6.6198706660591,-7.1157124131703,-1.));
#4998=CARTESIAN_POINT('Ctrl Pts',(6.60587239994885,-7.05836882883084,-1.));
#4999=CARTESIAN_POINT('Ctrl Pts',(6.5912030640433,-7.00141528186887,-1.));
#5000=CARTESIAN_POINT('Ctrl Pts',(6.5758359541656,-6.94488033148854,-1.));
#5001=CARTESIAN_POINT('Ctrl Pts',(6.55974857229919,-6.88878938806038,-1.));
#5002=CARTESIAN_POINT('Ctrl Pts',(6.54292981913303,-6.83315901897032,-1.));
#5003=CARTESIAN_POINT('Ctrl Pts',(6.52538888693355,-6.77798990345397,-1.));
#5004=CARTESIAN_POINT('Ctrl Pts',(6.50715912032692,-6.72326378902152,-1.));
#5005=CARTESIAN_POINT('Ctrl Pts',(6.48827758470622,-6.66895976394945,-1.));
#5006=CARTESIAN_POINT('Ctrl Pts',(6.46876645798848,-6.61506907935741,-1.));
#5007=CARTESIAN_POINT('Ctrl Pts',(6.44861636238489,-6.56160843323029,-1.));
#5008=CARTESIAN_POINT('Ctrl Pts',(6.42776254872513,-6.50863892931077,-1.));
#5009=CARTESIAN_POINT('Ctrl Pts',(6.40608444337877,-6.45626649182453,-1.));
#5010=CARTESIAN_POINT('Ctrl Pts',(6.38345478017075,-6.404602962683,-1.));
#5011=CARTESIAN_POINT('Ctrl Pts',(6.35978286360965,-6.35373180396277,-1.));
#5012=CARTESIAN_POINT('Ctrl Pts',(6.33505137069502,-6.30367904881887,-1.));
#5013=CARTESIAN_POINT('Ctrl Pts',(6.309377504208,-6.25436463761971,-1.));
#5014=CARTESIAN_POINT('Ctrl Pts',(6.28297985424307,-6.20562962932065,-1.));
#5015=CARTESIAN_POINT('Ctrl Pts',(6.25605474467853,-6.15733614814836,-1.));
#5016=CARTESIAN_POINT('Ctrl Pts',(6.22866991793491,-6.10945353793714,-1.));
#5017=CARTESIAN_POINT('Ctrl Pts',(6.20066685685754,-6.06213722636287,-1.));
#5018=CARTESIAN_POINT('Ctrl Pts',(6.17151878498998,-6.01584411654484,-1.));
#5019=CARTESIAN_POINT('Ctrl Pts',(6.14045331140033,-5.97123031969247,-1.));
#5020=CARTESIAN_POINT('Ctrl Pts',(6.11342775487885,-5.9374218385168,-1.));
#5021=CARTESIAN_POINT('Ctrl Pts',(6.09164867072823,-5.91336588048664,-1.));
#5022=CARTESIAN_POINT('Ctrl Pts',(6.07642118935899,-5.89793753402585,-1.));
#5023=CARTESIAN_POINT('Ctrl Pts',(6.06863042059311,-5.89037560471067,-1.));
#5024=CARTESIAN_POINT('',(6.60014603862874,-10.0218796774245,6.));
#5025=CARTESIAN_POINT('Ctrl Pts',(6.60014603862877,-10.0218796774244,6.));
#5026=CARTESIAN_POINT('Ctrl Pts',(6.60293150665658,-10.0085665785717,6.));
#5027=CARTESIAN_POINT('Ctrl Pts',(6.60844558393655,-9.98194823089969,6.));
#5028=CARTESIAN_POINT('Ctrl Pts',(6.61654612354182,-9.94204425953052,6.));
#5029=CARTESIAN_POINT('Ctrl Pts',(6.62700557693595,-9.88888607996273,6.));
#5030=CARTESIAN_POINT('Ctrl Pts',(6.63951038900666,-9.82251725114899,6.));
#5031=CARTESIAN_POINT('Ctrl Pts',(6.65144464725858,-9.75622826411014,6.));
#5032=CARTESIAN_POINT('Ctrl Pts',(6.66280711160719,-9.69002090483258,6.));
#5033=CARTESIAN_POINT('Ctrl Pts',(6.6735964736696,-9.62389802250188,6.));
#5034=CARTESIAN_POINT('Ctrl Pts',(6.68381150859182,-9.55786385494287,6.));
#5035=CARTESIAN_POINT('Ctrl Pts',(6.69345108162376,-9.49192378686254,6.));
#5036=CARTESIAN_POINT('Ctrl Pts',(6.70251410760818,-9.42608392519667,6.));
#5037=CARTESIAN_POINT('Ctrl Pts',(6.71099953007123,-9.36035072031877,6.));
#5038=CARTESIAN_POINT('Ctrl Pts',(6.71890629646186,-9.29473060155551,6.));
#5039=CARTESIAN_POINT('Ctrl Pts',(6.72623333926845,-9.22922952332026,6.));
#5040=CARTESIAN_POINT('Ctrl Pts',(6.73297955932547,-9.16385288053588,6.));
#5041=CARTESIAN_POINT('Ctrl Pts',(6.73914381348522,-9.09860577342166,6.));
#5042=CARTESIAN_POINT('Ctrl Pts',(6.74472490424422,-9.03349318036199,6.));
#5043=CARTESIAN_POINT('Ctrl Pts',(6.74972157399228,-8.96852015431047,6.));
#5044=CARTESIAN_POINT('Ctrl Pts',(6.75413249860575,-8.90369203916218,6.));
#5045=CARTESIAN_POINT('Ctrl Pts',(6.75795629519249,-8.83901457377472,6.));
#5046=CARTESIAN_POINT('Ctrl Pts',(6.76119155448274,-8.77449374557665,6.));
#5047=CARTESIAN_POINT('Ctrl Pts',(6.76383687353852,-8.710135693856,6.));
#5048=CARTESIAN_POINT('Ctrl Pts',(6.76589088878265,-8.64594659806299,6.));
#5049=CARTESIAN_POINT('Ctrl Pts',(6.76735232235634,-8.5819325577994,6.));
#5050=CARTESIAN_POINT('Ctrl Pts',(6.76822000004554,-8.51809951610774,6.));
#5051=CARTESIAN_POINT('Ctrl Pts',(6.76849272647565,-8.45445340444927,6.));
#5052=CARTESIAN_POINT('Ctrl Pts',(6.76816918165127,-8.39100025749019,6.));
#5053=CARTESIAN_POINT('Ctrl Pts',(6.76724781676281,-8.32774633509908,6.));
#5054=CARTESIAN_POINT('Ctrl Pts',(6.76572674650934,-8.26469824786603,6.));
#5055=CARTESIAN_POINT('Ctrl Pts',(6.76360366961639,-8.20186305794855,6.));
#5056=CARTESIAN_POINT('Ctrl Pts',(6.76087611417305,-8.13924806419108,6.));
#5057=CARTESIAN_POINT('Ctrl Pts',(6.75754166486089,-8.07686060726828,6.));
#5058=CARTESIAN_POINT('Ctrl Pts',(6.75359819949754,-8.01470786732019,6.));
#5059=CARTESIAN_POINT('Ctrl Pts',(6.7490441308376,-7.95279665937614,6.));
#5060=CARTESIAN_POINT('Ctrl Pts',(6.74387863902607,-7.89113323756913,6.));
#5061=CARTESIAN_POINT('Ctrl Pts',(6.73810106562748,-7.82972378407325,6.));
#5062=CARTESIAN_POINT('Ctrl Pts',(6.73171032576035,-7.76857488460784,6.));
#5063=CARTESIAN_POINT('Ctrl Pts',(6.72470431659336,-7.70769400824503,6.));
#5064=CARTESIAN_POINT('Ctrl Pts',(6.71707933277187,-7.6470899828899,6.));
#5065=CARTESIAN_POINT('Ctrl Pts',(6.70882947565317,-7.58677347699226,6.));
#5066=CARTESIAN_POINT('Ctrl Pts',(6.69994799095523,-7.52675593674633,6.));
#5067=CARTESIAN_POINT('Ctrl Pts',(6.69042862091103,-7.46704851290035,6.));
#5068=CARTESIAN_POINT('Ctrl Pts',(6.68026694677667,-7.40766099640558,6.));
#5069=CARTESIAN_POINT('Ctrl Pts',(6.66946176275797,-7.34860073021492,6.));
#5070=CARTESIAN_POINT('Ctrl Pts',(6.65801638970246,-7.28987157005224,6.));
#5071=CARTESIAN_POINT('Ctrl Pts',(6.64593535561052,-7.23147652896403,6.));
#5072=CARTESIAN_POINT('Ctrl Pts',(6.63322107969568,-7.17342042004756,6.));
#5073=CARTESIAN_POINT('Ctrl Pts',(6.6198706660591,-7.1157124131703,6.));
#5074=CARTESIAN_POINT('Ctrl Pts',(6.60587239994885,-7.05836882883084,6.));
#5075=CARTESIAN_POINT('Ctrl Pts',(6.5912030640433,-7.00141528186887,6.));
#5076=CARTESIAN_POINT('Ctrl Pts',(6.5758359541656,-6.94488033148854,6.));
#5077=CARTESIAN_POINT('Ctrl Pts',(6.55974857229919,-6.88878938806038,6.));
#5078=CARTESIAN_POINT('Ctrl Pts',(6.54292981913303,-6.83315901897032,6.));
#5079=CARTESIAN_POINT('Ctrl Pts',(6.52538888693355,-6.77798990345397,6.));
#5080=CARTESIAN_POINT('Ctrl Pts',(6.50715912032692,-6.72326378902152,6.));
#5081=CARTESIAN_POINT('Ctrl Pts',(6.48827758470622,-6.66895976394945,6.));
#5082=CARTESIAN_POINT('Ctrl Pts',(6.46876645798848,-6.61506907935741,6.));
#5083=CARTESIAN_POINT('Ctrl Pts',(6.44861636238489,-6.56160843323029,6.));
#5084=CARTESIAN_POINT('Ctrl Pts',(6.42776254872513,-6.50863892931077,6.));
#5085=CARTESIAN_POINT('Ctrl Pts',(6.40608444337877,-6.45626649182453,6.));
#5086=CARTESIAN_POINT('Ctrl Pts',(6.38345478017075,-6.404602962683,6.));
#5087=CARTESIAN_POINT('Ctrl Pts',(6.35978286360965,-6.35373180396277,6.));
#5088=CARTESIAN_POINT('Ctrl Pts',(6.33505137069502,-6.30367904881887,6.));
#5089=CARTESIAN_POINT('Ctrl Pts',(6.309377504208,-6.25436463761971,6.));
#5090=CARTESIAN_POINT('Ctrl Pts',(6.28297985424307,-6.20562962932065,6.));
#5091=CARTESIAN_POINT('Ctrl Pts',(6.25605474467853,-6.15733614814836,6.));
#5092=CARTESIAN_POINT('Ctrl Pts',(6.22866991793491,-6.10945353793714,6.));
#5093=CARTESIAN_POINT('Ctrl Pts',(6.20066685685754,-6.06213722636287,6.));
#5094=CARTESIAN_POINT('Ctrl Pts',(6.17151878498998,-6.01584411654484,6.));
#5095=CARTESIAN_POINT('Ctrl Pts',(6.14045331140033,-5.97123031969247,6.));
#5096=CARTESIAN_POINT('Ctrl Pts',(6.11342775487885,-5.9374218385168,6.));
#5097=CARTESIAN_POINT('Ctrl Pts',(6.09164867072823,-5.91336588048664,6.));
#5098=CARTESIAN_POINT('Ctrl Pts',(6.07642118935899,-5.89793753402585,6.));
#5099=CARTESIAN_POINT('Ctrl Pts',(6.06863042059311,-5.89037560471067,6.));
#5100=CARTESIAN_POINT('',(6.60014603862874,-10.0218796774245,0.));
#5101=CARTESIAN_POINT('Origin',(1.99840144432528E-13,-3.46133283549042E-13,
0.));
#5102=CARTESIAN_POINT('',(5.37912937500616,-10.726833976852,-1.));
#5103=CARTESIAN_POINT('Origin',(1.99840144432528E-13,-3.46133283549042E-13,
-1.));
#5104=CARTESIAN_POINT('',(5.37912937500616,-10.726833976852,6.));
#5105=CARTESIAN_POINT('Origin',(1.99840144432528E-13,-3.46133283549042E-13,
6.));
#5106=CARTESIAN_POINT('',(5.37912937500616,-10.726833976852,0.));
#5107=CARTESIAN_POINT('Ctrl Pts',(2.06689970121499,-8.20077591276801,-3.75));
#5108=CARTESIAN_POINT('Ctrl Pts',(2.06689970121499,-8.20077591276801,12.75));
#5109=CARTESIAN_POINT('Ctrl Pts',(2.06955313972063,-8.21130388109186,-3.75));
#5110=CARTESIAN_POINT('Ctrl Pts',(2.06955313972063,-8.21130388109186,12.75));
#5111=CARTESIAN_POINT('Ctrl Pts',(2.07530073900943,-8.23220544002367,-3.75));
#5112=CARTESIAN_POINT('Ctrl Pts',(2.07530073900943,-8.23220544002367,12.75));
#5113=CARTESIAN_POINT('Ctrl Pts',(2.08524426770062,-8.26309465918435,-3.75));
#5114=CARTESIAN_POINT('Ctrl Pts',(2.08524426770062,-8.26309465918435,12.75));
#5115=CARTESIAN_POINT('Ctrl Pts',(2.10101049300138,-8.3034037182712,-3.75));
#5116=CARTESIAN_POINT('Ctrl Pts',(2.10101049300138,-8.3034037182712,12.75));
#5117=CARTESIAN_POINT('Ctrl Pts',(2.12411443763998,-8.35261410600662,-3.75));
#5118=CARTESIAN_POINT('Ctrl Pts',(2.12411443763998,-8.35261410600662,12.75));
#5119=CARTESIAN_POINT('Ctrl Pts',(2.14963141082879,-8.40100363162428,-3.75));
#5120=CARTESIAN_POINT('Ctrl Pts',(2.14963141082879,-8.40100363162428,12.75));
#5121=CARTESIAN_POINT('Ctrl Pts',(2.17660700812681,-8.44891314968814,-3.75));
#5122=CARTESIAN_POINT('Ctrl Pts',(2.17660700812681,-8.44891314968814,12.75));
#5123=CARTESIAN_POINT('Ctrl Pts',(2.20438215159743,-8.49657041043196,-3.75));
#5124=CARTESIAN_POINT('Ctrl Pts',(2.20438215159743,-8.49657041043196,12.75));
#5125=CARTESIAN_POINT('Ctrl Pts',(2.23274297834755,-8.54403497990068,-3.75));
#5126=CARTESIAN_POINT('Ctrl Pts',(2.23274297834755,-8.54403497990068,12.75));
#5127=CARTESIAN_POINT('Ctrl Pts',(2.26174990860571,-8.59126351952005,-3.75));
#5128=CARTESIAN_POINT('Ctrl Pts',(2.26174990860571,-8.59126351952005,12.75));
#5129=CARTESIAN_POINT('Ctrl Pts',(2.29162050823335,-8.63815494571075,-3.75));
#5130=CARTESIAN_POINT('Ctrl Pts',(2.29162050823335,-8.63815494571075,12.75));
#5131=CARTESIAN_POINT('Ctrl Pts',(2.32260171926005,-8.68459942442029,-3.75));
#5132=CARTESIAN_POINT('Ctrl Pts',(2.32260171926005,-8.68459942442029,12.75));
#5133=CARTESIAN_POINT('Ctrl Pts',(2.35482147675117,-8.73053548487858,-3.75));
#5134=CARTESIAN_POINT('Ctrl Pts',(2.35482147675117,-8.73053548487858,12.75));
#5135=CARTESIAN_POINT('Ctrl Pts',(2.38824857383288,-8.77596511266658,-3.75));
#5136=CARTESIAN_POINT('Ctrl Pts',(2.38824857383288,-8.77596511266658,12.75));
#5137=CARTESIAN_POINT('Ctrl Pts',(2.4227653824809,-8.82092512134556,-3.75));
#5138=CARTESIAN_POINT('Ctrl Pts',(2.4227653824809,-8.82092512134556,12.75));
#5139=CARTESIAN_POINT('Ctrl Pts',(2.45821141167118,-8.86546980570045,-3.75));
#5140=CARTESIAN_POINT('Ctrl Pts',(2.45821141167118,-8.86546980570045,12.75));
#5141=CARTESIAN_POINT('Ctrl Pts',(2.4944346415182,-8.90965062344542,-3.75));
#5142=CARTESIAN_POINT('Ctrl Pts',(2.4944346415182,-8.90965062344542,12.75));
#5143=CARTESIAN_POINT('Ctrl Pts',(2.53134978004337,-8.95349309713545,-3.75));
#5144=CARTESIAN_POINT('Ctrl Pts',(2.53134978004337,-8.95349309713545,12.75));
#5145=CARTESIAN_POINT('Ctrl Pts',(2.56893767747318,-8.99699699918147,-3.75));
#5146=CARTESIAN_POINT('Ctrl Pts',(2.56893767747318,-8.99699699918147,12.75));
#5147=CARTESIAN_POINT('Ctrl Pts',(2.60721699951878,-9.0401474973841,-3.75));
#5148=CARTESIAN_POINT('Ctrl Pts',(2.60721699951878,-9.0401474973841,12.75));
#5149=CARTESIAN_POINT('Ctrl Pts',(2.64622438896051,-9.08292294803309,-3.75));
#5150=CARTESIAN_POINT('Ctrl Pts',(2.64622438896051,-9.08292294803309,12.75));
#5151=CARTESIAN_POINT('Ctrl Pts',(2.68599232523133,-9.12530360007999,-3.75));
#5152=CARTESIAN_POINT('Ctrl Pts',(2.68599232523133,-9.12530360007999,12.75));
#5153=CARTESIAN_POINT('Ctrl Pts',(2.72652481622915,-9.16728115317077,-3.75));
#5154=CARTESIAN_POINT('Ctrl Pts',(2.72652481622915,-9.16728115317077,12.75));
#5155=CARTESIAN_POINT('Ctrl Pts',(2.76780196452136,-9.20885693589776,-3.75));
#5156=CARTESIAN_POINT('Ctrl Pts',(2.76780196452136,-9.20885693589776,12.75));
#5157=CARTESIAN_POINT('Ctrl Pts',(2.80979051507329,-9.25003772692961,-3.75));
#5158=CARTESIAN_POINT('Ctrl Pts',(2.80979051507329,-9.25003772692961,12.75));
#5159=CARTESIAN_POINT('Ctrl Pts',(2.85245238280019,-9.29083237315975,-3.75));
#5160=CARTESIAN_POINT('Ctrl Pts',(2.85245238280019,-9.29083237315975,12.75));
#5161=CARTESIAN_POINT('Ctrl Pts',(2.89575377593937,-9.33124817395869,-3.75));
#5162=CARTESIAN_POINT('Ctrl Pts',(2.89575377593937,-9.33124817395869,12.75));
#5163=CARTESIAN_POINT('Ctrl Pts',(2.93967470314849,-9.3712871143499,-3.75));
#5164=CARTESIAN_POINT('Ctrl Pts',(2.93967470314849,-9.3712871143499,12.75));
#5165=CARTESIAN_POINT('Ctrl Pts',(2.98420577513995,-9.4109471173216,-3.75));
#5166=CARTESIAN_POINT('Ctrl Pts',(2.98420577513995,-9.4109471173216,12.75));
#5167=CARTESIAN_POINT('Ctrl Pts',(3.029344033256,-9.45022368122481,-3.75));
#5168=CARTESIAN_POINT('Ctrl Pts',(3.029344033256,-9.45022368122481,12.75));
#5169=CARTESIAN_POINT('Ctrl Pts',(3.07508913212203,-9.4891113781729,-3.75));
#5170=CARTESIAN_POINT('Ctrl Pts',(3.07508913212203,-9.4891113781729,12.75));
#5171=CARTESIAN_POINT('Ctrl Pts',(3.12143939300698,-9.52760540436562,-3.75));
#5172=CARTESIAN_POINT('Ctrl Pts',(3.12143939300698,-9.52760540436562,12.75));
#5173=CARTESIAN_POINT('Ctrl Pts',(3.16838785383003,-9.56570313257491,-3.75));
#5174=CARTESIAN_POINT('Ctrl Pts',(3.16838785383003,-9.56570313257491,12.75));
#5175=CARTESIAN_POINT('Ctrl Pts',(3.21592382600669,-9.60340349406962,-3.75));
#5176=CARTESIAN_POINT('Ctrl Pts',(3.21592382600669,-9.60340349406962,12.75));
#5177=CARTESIAN_POINT('Ctrl Pts',(3.26403452382221,-9.64070633286082,-3.75));
#5178=CARTESIAN_POINT('Ctrl Pts',(3.26403452382221,-9.64070633286082,12.75));
#5179=CARTESIAN_POINT('Ctrl Pts',(3.31270665744061,-9.67761177523124,-3.75));
#5180=CARTESIAN_POINT('Ctrl Pts',(3.31270665744061,-9.67761177523124,12.75));
#5181=CARTESIAN_POINT('Ctrl Pts',(3.36192803839196,-9.71411959533041,-3.75));
#5182=CARTESIAN_POINT('Ctrl Pts',(3.36192803839196,-9.71411959533041,12.75));
#5183=CARTESIAN_POINT('Ctrl Pts',(3.4116891688089,-9.75022858813702,-3.75));
#5184=CARTESIAN_POINT('Ctrl Pts',(3.4116891688089,-9.75022858813702,12.75));
#5185=CARTESIAN_POINT('Ctrl Pts',(3.46198252886956,-9.78593684022038,-3.75));
#5186=CARTESIAN_POINT('Ctrl Pts',(3.46198252886956,-9.78593684022038,12.75));
#5187=CARTESIAN_POINT('Ctrl Pts',(3.51280187273294,-9.8212419982557,-3.75));
#5188=CARTESIAN_POINT('Ctrl Pts',(3.51280187273294,-9.8212419982557,12.75));
#5189=CARTESIAN_POINT('Ctrl Pts',(3.5641415172615,-9.85614154137781,-3.75));
#5190=CARTESIAN_POINT('Ctrl Pts',(3.5641415172615,-9.85614154137781,12.75));
#5191=CARTESIAN_POINT('Ctrl Pts',(3.61599563628968,-9.89063305253546,-3.75));
#5192=CARTESIAN_POINT('Ctrl Pts',(3.61599563628968,-9.89063305253546,12.75));
#5193=CARTESIAN_POINT('Ctrl Pts',(3.66835753420625,-9.92471449880883,-3.75));
#5194=CARTESIAN_POINT('Ctrl Pts',(3.66835753420625,-9.92471449880883,12.75));
#5195=CARTESIAN_POINT('Ctrl Pts',(3.72121993173636,-9.95838412799173,-3.75));
#5196=CARTESIAN_POINT('Ctrl Pts',(3.72121993173636,-9.95838412799173,12.75));
#5197=CARTESIAN_POINT('Ctrl Pts',(3.77457526401003,-9.99164036147395,-3.75));
#5198=CARTESIAN_POINT('Ctrl Pts',(3.77457526401003,-9.99164036147395,12.75));
#5199=CARTESIAN_POINT('Ctrl Pts',(3.82841597408714,-10.0244816905709,-3.75));
#5200=CARTESIAN_POINT('Ctrl Pts',(3.82841597408714,-10.0244816905709,12.75));
#5201=CARTESIAN_POINT('Ctrl Pts',(3.88273479532262,-10.056906577166,-3.75));
#5202=CARTESIAN_POINT('Ctrl Pts',(3.88273479532262,-10.056906577166,12.75));
#5203=CARTESIAN_POINT('Ctrl Pts',(3.93752506012706,-10.0889133486827,-3.75));
#5204=CARTESIAN_POINT('Ctrl Pts',(3.93752506012706,-10.0889133486827,12.75));
#5205=CARTESIAN_POINT('Ctrl Pts',(3.99278057289045,-10.1205002164952,-3.75));
#5206=CARTESIAN_POINT('Ctrl Pts',(3.99278057289045,-10.1205002164952,12.75));
#5207=CARTESIAN_POINT('Ctrl Pts',(4.04849544744086,-10.1516653064199,-3.75));
#5208=CARTESIAN_POINT('Ctrl Pts',(4.04849544744086,-10.1516653064199,12.75));
#5209=CARTESIAN_POINT('Ctrl Pts',(4.10466394929485,-10.1824066879509,-3.75));
#5210=CARTESIAN_POINT('Ctrl Pts',(4.10466394929485,-10.1824066879509,12.75));
#5211=CARTESIAN_POINT('Ctrl Pts',(4.16128034451961,-10.2127224064663,-3.75));
#5212=CARTESIAN_POINT('Ctrl Pts',(4.16128034451961,-10.2127224064663,12.75));
#5213=CARTESIAN_POINT('Ctrl Pts',(4.21833871177566,-10.2426105188232,-3.75));
#5214=CARTESIAN_POINT('Ctrl Pts',(4.21833871177566,-10.2426105188232,12.75));
#5215=CARTESIAN_POINT('Ctrl Pts',(4.27583301771352,-10.272069116189,-3.75));
#5216=CARTESIAN_POINT('Ctrl Pts',(4.27583301771352,-10.272069116189,12.75));
#5217=CARTESIAN_POINT('Ctrl Pts',(4.33375724408483,-10.3010963438997,-3.75));
#5218=CARTESIAN_POINT('Ctrl Pts',(4.33375724408483,-10.3010963438997,12.75));
#5219=CARTESIAN_POINT('Ctrl Pts',(4.39210550098944,-10.3296904287044,-3.75));
#5220=CARTESIAN_POINT('Ctrl Pts',(4.39210550098944,-10.3296904287044,12.75));
#5221=CARTESIAN_POINT('Ctrl Pts',(4.45087212698484,-10.3578496987941,-3.75));
#5222=CARTESIAN_POINT('Ctrl Pts',(4.45087212698484,-10.3578496987941,12.75));
#5223=CARTESIAN_POINT('Ctrl Pts',(4.51005183206029,-10.3855726289458,-3.75));
#5224=CARTESIAN_POINT('Ctrl Pts',(4.51005183206029,-10.3855726289458,12.75));
#5225=CARTESIAN_POINT('Ctrl Pts',(4.56963961142453,-10.4128577818052,-3.75));
#5226=CARTESIAN_POINT('Ctrl Pts',(4.56963961142453,-10.4128577818052,12.75));
#5227=CARTESIAN_POINT('Ctrl Pts',(4.62963055491845,-10.4397037052485,-3.75));
#5228=CARTESIAN_POINT('Ctrl Pts',(4.62963055491845,-10.4397037052485,12.75));
#5229=CARTESIAN_POINT('Ctrl Pts',(4.69001967404874,-10.466108839161,-3.75));
#5230=CARTESIAN_POINT('Ctrl Pts',(4.69001967404874,-10.466108839161,12.75));
#5231=CARTESIAN_POINT('Ctrl Pts',(4.75080174709239,-10.4920714379865,-3.75));
#5232=CARTESIAN_POINT('Ctrl Pts',(4.75080174709239,-10.4920714379865,12.75));
#5233=CARTESIAN_POINT('Ctrl Pts',(4.81197108362034,-10.5175894490106,-3.75));
#5234=CARTESIAN_POINT('Ctrl Pts',(4.81197108362034,-10.5175894490106,12.75));
#5235=CARTESIAN_POINT('Ctrl Pts',(4.87352158939685,-10.5426605691059,-3.75));
#5236=CARTESIAN_POINT('Ctrl Pts',(4.87352158939685,-10.5426605691059,12.75));
#5237=CARTESIAN_POINT('Ctrl Pts',(4.93544714999767,-10.5672824880187,-3.75));
#5238=CARTESIAN_POINT('Ctrl Pts',(4.93544714999767,-10.5672824880187,12.75));
#5239=CARTESIAN_POINT('Ctrl Pts',(4.99774193408263,-10.5914530920551,-3.75));
#5240=CARTESIAN_POINT('Ctrl Pts',(4.99774193408263,-10.5914530920551,12.75));
#5241=CARTESIAN_POINT('Ctrl Pts',(5.06040071098368,-10.6151706715837,-3.75));
#5242=CARTESIAN_POINT('Ctrl Pts',(5.06040071098368,-10.6151706715837,12.75));
#5243=CARTESIAN_POINT('Ctrl Pts',(5.12341919820983,-10.638434168447,-3.75));
#5244=CARTESIAN_POINT('Ctrl Pts',(5.12341919820983,-10.638434168447,12.75));
#5245=CARTESIAN_POINT('Ctrl Pts',(5.18679427410257,-10.661243291145,-3.75));
#5246=CARTESIAN_POINT('Ctrl Pts',(5.18679427410257,-10.661243291145,12.75));
#5247=CARTESIAN_POINT('Ctrl Pts',(5.25052377191005,-10.6835982206291,-3.75));
#5248=CARTESIAN_POINT('Ctrl Pts',(5.25052377191005,-10.6835982206291,12.75));
#5249=CARTESIAN_POINT('Ctrl Pts',(5.30178983253175,-10.7011191580639,-3.75));
#5250=CARTESIAN_POINT('Ctrl Pts',(5.30178983253175,-10.7011191580639,12.75));
#5251=CARTESIAN_POINT('Ctrl Pts',(5.34039795525197,-10.714055870666,-3.75));
#5252=CARTESIAN_POINT('Ctrl Pts',(5.34039795525197,-10.714055870666,12.75));
#5253=CARTESIAN_POINT('Ctrl Pts',(5.3662071591827,-10.7225897134991,-3.75));
#5254=CARTESIAN_POINT('Ctrl Pts',(5.3662071591827,-10.7225897134991,12.75));
#5255=CARTESIAN_POINT('Ctrl Pts',(5.37912937500616,-10.726833976852,-3.75));
#5256=CARTESIAN_POINT('Ctrl Pts',(5.37912937500616,-10.726833976852,12.75));
#5257=CARTESIAN_POINT('Ctrl Pts',(2.06689970121499,-8.20077591276801,-1.));
#5258=CARTESIAN_POINT('Ctrl Pts',(2.06955313972063,-8.21130388109186,-1.));
#5259=CARTESIAN_POINT('Ctrl Pts',(2.07530073900943,-8.23220544002367,-1.));
#5260=CARTESIAN_POINT('Ctrl Pts',(2.08524426770062,-8.26309465918435,-1.));
#5261=CARTESIAN_POINT('Ctrl Pts',(2.10101049300138,-8.3034037182712,-1.));
#5262=CARTESIAN_POINT('Ctrl Pts',(2.12411443763998,-8.35261410600662,-1.));
#5263=CARTESIAN_POINT('Ctrl Pts',(2.14963141082879,-8.40100363162428,-1.));
#5264=CARTESIAN_POINT('Ctrl Pts',(2.17660700812681,-8.44891314968814,-1.));
#5265=CARTESIAN_POINT('Ctrl Pts',(2.20438215159743,-8.49657041043196,-1.));
#5266=CARTESIAN_POINT('Ctrl Pts',(2.23274297834755,-8.54403497990068,-1.));
#5267=CARTESIAN_POINT('Ctrl Pts',(2.26174990860571,-8.59126351952005,-1.));
#5268=CARTESIAN_POINT('Ctrl Pts',(2.29162050823335,-8.63815494571075,-1.));
#5269=CARTESIAN_POINT('Ctrl Pts',(2.32260171926005,-8.68459942442029,-1.));
#5270=CARTESIAN_POINT('Ctrl Pts',(2.35482147675117,-8.73053548487858,-1.));
#5271=CARTESIAN_POINT('Ctrl Pts',(2.38824857383288,-8.77596511266658,-1.));
#5272=CARTESIAN_POINT('Ctrl Pts',(2.4227653824809,-8.82092512134556,-1.));
#5273=CARTESIAN_POINT('Ctrl Pts',(2.45821141167118,-8.86546980570045,-1.));
#5274=CARTESIAN_POINT('Ctrl Pts',(2.4944346415182,-8.90965062344542,-1.));
#5275=CARTESIAN_POINT('Ctrl Pts',(2.53134978004337,-8.95349309713545,-1.));
#5276=CARTESIAN_POINT('Ctrl Pts',(2.56893767747318,-8.99699699918147,-1.));
#5277=CARTESIAN_POINT('Ctrl Pts',(2.60721699951878,-9.0401474973841,-1.));
#5278=CARTESIAN_POINT('Ctrl Pts',(2.64622438896051,-9.08292294803309,-1.));
#5279=CARTESIAN_POINT('Ctrl Pts',(2.68599232523133,-9.12530360007999,-1.));
#5280=CARTESIAN_POINT('Ctrl Pts',(2.72652481622915,-9.16728115317077,-1.));
#5281=CARTESIAN_POINT('Ctrl Pts',(2.76780196452136,-9.20885693589776,-1.));
#5282=CARTESIAN_POINT('Ctrl Pts',(2.80979051507329,-9.25003772692961,-1.));
#5283=CARTESIAN_POINT('Ctrl Pts',(2.85245238280019,-9.29083237315975,-1.));
#5284=CARTESIAN_POINT('Ctrl Pts',(2.89575377593937,-9.33124817395869,-1.));
#5285=CARTESIAN_POINT('Ctrl Pts',(2.93967470314849,-9.3712871143499,-1.));
#5286=CARTESIAN_POINT('Ctrl Pts',(2.98420577513995,-9.4109471173216,-1.));
#5287=CARTESIAN_POINT('Ctrl Pts',(3.029344033256,-9.45022368122481,-1.));
#5288=CARTESIAN_POINT('Ctrl Pts',(3.07508913212203,-9.4891113781729,-1.));
#5289=CARTESIAN_POINT('Ctrl Pts',(3.12143939300698,-9.52760540436562,-1.));
#5290=CARTESIAN_POINT('Ctrl Pts',(3.16838785383003,-9.56570313257491,-1.));
#5291=CARTESIAN_POINT('Ctrl Pts',(3.21592382600669,-9.60340349406962,-1.));
#5292=CARTESIAN_POINT('Ctrl Pts',(3.26403452382221,-9.64070633286082,-1.));
#5293=CARTESIAN_POINT('Ctrl Pts',(3.31270665744061,-9.67761177523124,-1.));
#5294=CARTESIAN_POINT('Ctrl Pts',(3.36192803839196,-9.71411959533041,-1.));
#5295=CARTESIAN_POINT('Ctrl Pts',(3.4116891688089,-9.75022858813702,-1.));
#5296=CARTESIAN_POINT('Ctrl Pts',(3.46198252886956,-9.78593684022038,-1.));
#5297=CARTESIAN_POINT('Ctrl Pts',(3.51280187273294,-9.8212419982557,-1.));
#5298=CARTESIAN_POINT('Ctrl Pts',(3.5641415172615,-9.85614154137781,-1.));
#5299=CARTESIAN_POINT('Ctrl Pts',(3.61599563628968,-9.89063305253546,-1.));
#5300=CARTESIAN_POINT('Ctrl Pts',(3.66835753420625,-9.92471449880883,-1.));
#5301=CARTESIAN_POINT('Ctrl Pts',(3.72121993173636,-9.95838412799173,-1.));
#5302=CARTESIAN_POINT('Ctrl Pts',(3.77457526401003,-9.99164036147395,-1.));
#5303=CARTESIAN_POINT('Ctrl Pts',(3.82841597408714,-10.0244816905709,-1.));
#5304=CARTESIAN_POINT('Ctrl Pts',(3.88273479532262,-10.056906577166,-1.));
#5305=CARTESIAN_POINT('Ctrl Pts',(3.93752506012706,-10.0889133486827,-1.));
#5306=CARTESIAN_POINT('Ctrl Pts',(3.99278057289045,-10.1205002164952,-1.));
#5307=CARTESIAN_POINT('Ctrl Pts',(4.04849544744086,-10.1516653064199,-1.));
#5308=CARTESIAN_POINT('Ctrl Pts',(4.10466394929485,-10.1824066879509,-1.));
#5309=CARTESIAN_POINT('Ctrl Pts',(4.16128034451961,-10.2127224064663,-1.));
#5310=CARTESIAN_POINT('Ctrl Pts',(4.21833871177566,-10.2426105188232,-1.));
#5311=CARTESIAN_POINT('Ctrl Pts',(4.27583301771352,-10.272069116189,-1.));
#5312=CARTESIAN_POINT('Ctrl Pts',(4.33375724408483,-10.3010963438997,-1.));
#5313=CARTESIAN_POINT('Ctrl Pts',(4.39210550098944,-10.3296904287044,-1.));
#5314=CARTESIAN_POINT('Ctrl Pts',(4.45087212698484,-10.3578496987941,-1.));
#5315=CARTESIAN_POINT('Ctrl Pts',(4.51005183206029,-10.3855726289458,-1.));
#5316=CARTESIAN_POINT('Ctrl Pts',(4.56963961142453,-10.4128577818052,-1.));
#5317=CARTESIAN_POINT('Ctrl Pts',(4.62963055491845,-10.4397037052485,-1.));
#5318=CARTESIAN_POINT('Ctrl Pts',(4.69001967404874,-10.466108839161,-1.));
#5319=CARTESIAN_POINT('Ctrl Pts',(4.75080174709239,-10.4920714379865,-1.));
#5320=CARTESIAN_POINT('Ctrl Pts',(4.81197108362034,-10.5175894490106,-1.));
#5321=CARTESIAN_POINT('Ctrl Pts',(4.87352158939685,-10.5426605691059,-1.));
#5322=CARTESIAN_POINT('Ctrl Pts',(4.93544714999767,-10.5672824880187,-1.));
#5323=CARTESIAN_POINT('Ctrl Pts',(4.99774193408263,-10.5914530920551,-1.));
#5324=CARTESIAN_POINT('Ctrl Pts',(5.06040071098368,-10.6151706715837,-1.));
#5325=CARTESIAN_POINT('Ctrl Pts',(5.12341919820983,-10.638434168447,-1.));
#5326=CARTESIAN_POINT('Ctrl Pts',(5.18679427410257,-10.661243291145,-1.));
#5327=CARTESIAN_POINT('Ctrl Pts',(5.25052377191005,-10.6835982206291,-1.));
#5328=CARTESIAN_POINT('Ctrl Pts',(5.30178983253175,-10.7011191580639,-1.));
#5329=CARTESIAN_POINT('Ctrl Pts',(5.34039795525197,-10.714055870666,-1.));
#5330=CARTESIAN_POINT('Ctrl Pts',(5.3662071591827,-10.7225897134991,-1.));
#5331=CARTESIAN_POINT('Ctrl Pts',(5.37912937500616,-10.726833976852,-1.));
#5332=CARTESIAN_POINT('Ctrl Pts',(2.06689970121499,-8.20077591276801,6.));
#5333=CARTESIAN_POINT('Ctrl Pts',(2.06955313972063,-8.21130388109186,6.));
#5334=CARTESIAN_POINT('Ctrl Pts',(2.07530073900943,-8.23220544002367,6.));
#5335=CARTESIAN_POINT('Ctrl Pts',(2.08524426770062,-8.26309465918435,6.));
#5336=CARTESIAN_POINT('Ctrl Pts',(2.10101049300138,-8.3034037182712,6.));
#5337=CARTESIAN_POINT('Ctrl Pts',(2.12411443763998,-8.35261410600662,6.));
#5338=CARTESIAN_POINT('Ctrl Pts',(2.14963141082879,-8.40100363162428,6.));
#5339=CARTESIAN_POINT('Ctrl Pts',(2.17660700812681,-8.44891314968814,6.));
#5340=CARTESIAN_POINT('Ctrl Pts',(2.20438215159743,-8.49657041043196,6.));
#5341=CARTESIAN_POINT('Ctrl Pts',(2.23274297834755,-8.54403497990068,6.));
#5342=CARTESIAN_POINT('Ctrl Pts',(2.26174990860571,-8.59126351952005,6.));
#5343=CARTESIAN_POINT('Ctrl Pts',(2.29162050823335,-8.63815494571075,6.));
#5344=CARTESIAN_POINT('Ctrl Pts',(2.32260171926005,-8.68459942442029,6.));
#5345=CARTESIAN_POINT('Ctrl Pts',(2.35482147675117,-8.73053548487858,6.));
#5346=CARTESIAN_POINT('Ctrl Pts',(2.38824857383288,-8.77596511266658,6.));
#5347=CARTESIAN_POINT('Ctrl Pts',(2.4227653824809,-8.82092512134556,6.));
#5348=CARTESIAN_POINT('Ctrl Pts',(2.45821141167118,-8.86546980570045,6.));
#5349=CARTESIAN_POINT('Ctrl Pts',(2.4944346415182,-8.90965062344542,6.));
#5350=CARTESIAN_POINT('Ctrl Pts',(2.53134978004337,-8.95349309713545,6.));
#5351=CARTESIAN_POINT('Ctrl Pts',(2.56893767747318,-8.99699699918147,6.));
#5352=CARTESIAN_POINT('Ctrl Pts',(2.60721699951878,-9.0401474973841,6.));
#5353=CARTESIAN_POINT('Ctrl Pts',(2.64622438896051,-9.08292294803309,6.));
#5354=CARTESIAN_POINT('Ctrl Pts',(2.68599232523133,-9.12530360007999,6.));
#5355=CARTESIAN_POINT('Ctrl Pts',(2.72652481622915,-9.16728115317077,6.));
#5356=CARTESIAN_POINT('Ctrl Pts',(2.76780196452136,-9.20885693589776,6.));
#5357=CARTESIAN_POINT('Ctrl Pts',(2.80979051507329,-9.25003772692961,6.));
#5358=CARTESIAN_POINT('Ctrl Pts',(2.85245238280019,-9.29083237315975,6.));
#5359=CARTESIAN_POINT('Ctrl Pts',(2.89575377593937,-9.33124817395869,6.));
#5360=CARTESIAN_POINT('Ctrl Pts',(2.93967470314849,-9.3712871143499,6.));
#5361=CARTESIAN_POINT('Ctrl Pts',(2.98420577513995,-9.4109471173216,6.));
#5362=CARTESIAN_POINT('Ctrl Pts',(3.029344033256,-9.45022368122481,6.));
#5363=CARTESIAN_POINT('Ctrl Pts',(3.07508913212203,-9.4891113781729,6.));
#5364=CARTESIAN_POINT('Ctrl Pts',(3.12143939300698,-9.52760540436562,6.));
#5365=CARTESIAN_POINT('Ctrl Pts',(3.16838785383003,-9.56570313257491,6.));
#5366=CARTESIAN_POINT('Ctrl Pts',(3.21592382600669,-9.60340349406962,6.));
#5367=CARTESIAN_POINT('Ctrl Pts',(3.26403452382221,-9.64070633286082,6.));
#5368=CARTESIAN_POINT('Ctrl Pts',(3.31270665744061,-9.67761177523124,6.));
#5369=CARTESIAN_POINT('Ctrl Pts',(3.36192803839196,-9.71411959533041,6.));
#5370=CARTESIAN_POINT('Ctrl Pts',(3.4116891688089,-9.75022858813702,6.));
#5371=CARTESIAN_POINT('Ctrl Pts',(3.46198252886956,-9.78593684022038,6.));
#5372=CARTESIAN_POINT('Ctrl Pts',(3.51280187273294,-9.8212419982557,6.));
#5373=CARTESIAN_POINT('Ctrl Pts',(3.5641415172615,-9.85614154137781,6.));
#5374=CARTESIAN_POINT('Ctrl Pts',(3.61599563628968,-9.89063305253546,6.));
#5375=CARTESIAN_POINT('Ctrl Pts',(3.66835753420625,-9.92471449880883,6.));
#5376=CARTESIAN_POINT('Ctrl Pts',(3.72121993173636,-9.95838412799173,6.));
#5377=CARTESIAN_POINT('Ctrl Pts',(3.77457526401003,-9.99164036147395,6.));
#5378=CARTESIAN_POINT('Ctrl Pts',(3.82841597408714,-10.0244816905709,6.));
#5379=CARTESIAN_POINT('Ctrl Pts',(3.88273479532262,-10.056906577166,6.));
#5380=CARTESIAN_POINT('Ctrl Pts',(3.93752506012706,-10.0889133486827,6.));
#5381=CARTESIAN_POINT('Ctrl Pts',(3.99278057289045,-10.1205002164952,6.));
#5382=CARTESIAN_POINT('Ctrl Pts',(4.04849544744086,-10.1516653064199,6.));
#5383=CARTESIAN_POINT('Ctrl Pts',(4.10466394929485,-10.1824066879509,6.));
#5384=CARTESIAN_POINT('Ctrl Pts',(4.16128034451961,-10.2127224064663,6.));
#5385=CARTESIAN_POINT('Ctrl Pts',(4.21833871177566,-10.2426105188232,6.));
#5386=CARTESIAN_POINT('Ctrl Pts',(4.27583301771352,-10.272069116189,6.));
#5387=CARTESIAN_POINT('Ctrl Pts',(4.33375724408483,-10.3010963438997,6.));
#5388=CARTESIAN_POINT('Ctrl Pts',(4.39210550098944,-10.3296904287044,6.));
#5389=CARTESIAN_POINT('Ctrl Pts',(4.45087212698484,-10.3578496987941,6.));
#5390=CARTESIAN_POINT('Ctrl Pts',(4.51005183206029,-10.3855726289458,6.));
#5391=CARTESIAN_POINT('Ctrl Pts',(4.56963961142453,-10.4128577818052,6.));
#5392=CARTESIAN_POINT('Ctrl Pts',(4.62963055491845,-10.4397037052485,6.));
#5393=CARTESIAN_POINT('Ctrl Pts',(4.69001967404874,-10.466108839161,6.));
#5394=CARTESIAN_POINT('Ctrl Pts',(4.75080174709239,-10.4920714379865,6.));
#5395=CARTESIAN_POINT('Ctrl Pts',(4.81197108362034,-10.5175894490106,6.));
#5396=CARTESIAN_POINT('Ctrl Pts',(4.87352158939685,-10.5426605691059,6.));
#5397=CARTESIAN_POINT('Ctrl Pts',(4.93544714999767,-10.5672824880187,6.));
#5398=CARTESIAN_POINT('Ctrl Pts',(4.99774193408263,-10.5914530920551,6.));
#5399=CARTESIAN_POINT('Ctrl Pts',(5.06040071098368,-10.6151706715837,6.));
#5400=CARTESIAN_POINT('Ctrl Pts',(5.12341919820983,-10.638434168447,6.));
#5401=CARTESIAN_POINT('Ctrl Pts',(5.18679427410257,-10.661243291145,6.));
#5402=CARTESIAN_POINT('Ctrl Pts',(5.25052377191005,-10.6835982206291,6.));
#5403=CARTESIAN_POINT('Ctrl Pts',(5.30178983253175,-10.7011191580639,6.));
#5404=CARTESIAN_POINT('Ctrl Pts',(5.34039795525197,-10.714055870666,6.));
#5405=CARTESIAN_POINT('Ctrl Pts',(5.3662071591827,-10.7225897134991,6.));
#5406=CARTESIAN_POINT('Ctrl Pts',(5.37912937500616,-10.726833976852,6.));
#5407=CARTESIAN_POINT('Ctrl Pts',(-5.37912937500618,-10.726833976852,-3.75));
#5408=CARTESIAN_POINT('Ctrl Pts',(-5.37912937500618,-10.726833976852,12.75));
#5409=CARTESIAN_POINT('Ctrl Pts',(-5.36620715918271,-10.7225897134991,-3.75));
#5410=CARTESIAN_POINT('Ctrl Pts',(-5.36620715918271,-10.7225897134991,12.75));
#5411=CARTESIAN_POINT('Ctrl Pts',(-5.34039795525199,-10.714055870666,-3.75));
#5412=CARTESIAN_POINT('Ctrl Pts',(-5.34039795525199,-10.714055870666,12.75));
#5413=CARTESIAN_POINT('Ctrl Pts',(-5.30178983253177,-10.7011191580639,-3.75));
#5414=CARTESIAN_POINT('Ctrl Pts',(-5.30178983253177,-10.7011191580639,12.75));
#5415=CARTESIAN_POINT('Ctrl Pts',(-5.25052377191006,-10.6835982206291,-3.75));
#5416=CARTESIAN_POINT('Ctrl Pts',(-5.25052377191006,-10.6835982206291,12.75));
#5417=CARTESIAN_POINT('Ctrl Pts',(-5.18679427410258,-10.661243291145,-3.75));
#5418=CARTESIAN_POINT('Ctrl Pts',(-5.18679427410258,-10.661243291145,12.75));
#5419=CARTESIAN_POINT('Ctrl Pts',(-5.12341919820984,-10.638434168447,-3.75));
#5420=CARTESIAN_POINT('Ctrl Pts',(-5.12341919820984,-10.638434168447,12.75));
#5421=CARTESIAN_POINT('Ctrl Pts',(-5.06040071098369,-10.6151706715837,-3.75));
#5422=CARTESIAN_POINT('Ctrl Pts',(-5.06040071098369,-10.6151706715837,12.75));
#5423=CARTESIAN_POINT('Ctrl Pts',(-4.99774193408265,-10.5914530920551,-3.75));
#5424=CARTESIAN_POINT('Ctrl Pts',(-4.99774193408265,-10.5914530920551,12.75));
#5425=CARTESIAN_POINT('Ctrl Pts',(-4.93544714999768,-10.5672824880187,-3.75));
#5426=CARTESIAN_POINT('Ctrl Pts',(-4.93544714999768,-10.5672824880187,12.75));
#5427=CARTESIAN_POINT('Ctrl Pts',(-4.87352158939686,-10.5426605691059,-3.75));
#5428=CARTESIAN_POINT('Ctrl Pts',(-4.87352158939686,-10.5426605691059,12.75));
#5429=CARTESIAN_POINT('Ctrl Pts',(-4.81197108362036,-10.5175894490106,-3.75));
#5430=CARTESIAN_POINT('Ctrl Pts',(-4.81197108362036,-10.5175894490106,12.75));
#5431=CARTESIAN_POINT('Ctrl Pts',(-4.7508017470924,-10.4920714379865,-3.75));
#5432=CARTESIAN_POINT('Ctrl Pts',(-4.7508017470924,-10.4920714379865,12.75));
#5433=CARTESIAN_POINT('Ctrl Pts',(-4.69001967404875,-10.4661088391609,-3.75));
#5434=CARTESIAN_POINT('Ctrl Pts',(-4.69001967404875,-10.4661088391609,12.75));
#5435=CARTESIAN_POINT('Ctrl Pts',(-4.62963055491846,-10.4397037052484,-3.75));
#5436=CARTESIAN_POINT('Ctrl Pts',(-4.62963055491846,-10.4397037052484,12.75));
#5437=CARTESIAN_POINT('Ctrl Pts',(-4.56963961142454,-10.4128577818052,-3.75));
#5438=CARTESIAN_POINT('Ctrl Pts',(-4.56963961142454,-10.4128577818052,12.75));
#5439=CARTESIAN_POINT('Ctrl Pts',(-4.5100518320603,-10.3855726289458,-3.75));
#5440=CARTESIAN_POINT('Ctrl Pts',(-4.5100518320603,-10.3855726289458,12.75));
#5441=CARTESIAN_POINT('Ctrl Pts',(-4.45087212698486,-10.3578496987941,-3.75));
#5442=CARTESIAN_POINT('Ctrl Pts',(-4.45087212698486,-10.3578496987941,12.75));
#5443=CARTESIAN_POINT('Ctrl Pts',(-4.39210550098945,-10.3296904287044,-3.75));
#5444=CARTESIAN_POINT('Ctrl Pts',(-4.39210550098945,-10.3296904287044,12.75));
#5445=CARTESIAN_POINT('Ctrl Pts',(-4.33375724408484,-10.3010963438997,-3.75));
#5446=CARTESIAN_POINT('Ctrl Pts',(-4.33375724408484,-10.3010963438997,12.75));
#5447=CARTESIAN_POINT('Ctrl Pts',(-4.27583301771354,-10.272069116189,-3.75));
#5448=CARTESIAN_POINT('Ctrl Pts',(-4.27583301771354,-10.272069116189,12.75));
#5449=CARTESIAN_POINT('Ctrl Pts',(-4.21833871177567,-10.2426105188232,-3.75));
#5450=CARTESIAN_POINT('Ctrl Pts',(-4.21833871177567,-10.2426105188232,12.75));
#5451=CARTESIAN_POINT('Ctrl Pts',(-4.16128034451963,-10.2127224064663,-3.75));
#5452=CARTESIAN_POINT('Ctrl Pts',(-4.16128034451963,-10.2127224064663,12.75));
#5453=CARTESIAN_POINT('Ctrl Pts',(-4.10466394929486,-10.1824066879509,-3.75));
#5454=CARTESIAN_POINT('Ctrl Pts',(-4.10466394929486,-10.1824066879509,12.75));
#5455=CARTESIAN_POINT('Ctrl Pts',(-4.04849544744087,-10.1516653064199,-3.75));
#5456=CARTESIAN_POINT('Ctrl Pts',(-4.04849544744087,-10.1516653064199,12.75));
#5457=CARTESIAN_POINT('Ctrl Pts',(-3.99278057289047,-10.1205002164952,-3.75));
#5458=CARTESIAN_POINT('Ctrl Pts',(-3.99278057289047,-10.1205002164952,12.75));
#5459=CARTESIAN_POINT('Ctrl Pts',(-3.93752506012707,-10.0889133486827,-3.75));
#5460=CARTESIAN_POINT('Ctrl Pts',(-3.93752506012707,-10.0889133486827,12.75));
#5461=CARTESIAN_POINT('Ctrl Pts',(-3.88273479532263,-10.056906577166,-3.75));
#5462=CARTESIAN_POINT('Ctrl Pts',(-3.88273479532263,-10.056906577166,12.75));
#5463=CARTESIAN_POINT('Ctrl Pts',(-3.82841597408715,-10.0244816905709,-3.75));
#5464=CARTESIAN_POINT('Ctrl Pts',(-3.82841597408715,-10.0244816905709,12.75));
#5465=CARTESIAN_POINT('Ctrl Pts',(-3.77457526401005,-9.99164036147395,-3.75));
#5466=CARTESIAN_POINT('Ctrl Pts',(-3.77457526401005,-9.99164036147395,12.75));
#5467=CARTESIAN_POINT('Ctrl Pts',(-3.72121993173637,-9.95838412799172,-3.75));
#5468=CARTESIAN_POINT('Ctrl Pts',(-3.72121993173637,-9.95838412799172,12.75));
#5469=CARTESIAN_POINT('Ctrl Pts',(-3.66835753420626,-9.92471449880882,-3.75));
#5470=CARTESIAN_POINT('Ctrl Pts',(-3.66835753420626,-9.92471449880882,12.75));
#5471=CARTESIAN_POINT('Ctrl Pts',(-3.61599563628969,-9.89063305253546,-3.75));
#5472=CARTESIAN_POINT('Ctrl Pts',(-3.61599563628969,-9.89063305253546,12.75));
#5473=CARTESIAN_POINT('Ctrl Pts',(-3.56414151726151,-9.8561415413778,-3.75));
#5474=CARTESIAN_POINT('Ctrl Pts',(-3.56414151726151,-9.8561415413778,12.75));
#5475=CARTESIAN_POINT('Ctrl Pts',(-3.51280187273296,-9.8212419982557,-3.75));
#5476=CARTESIAN_POINT('Ctrl Pts',(-3.51280187273296,-9.8212419982557,12.75));
#5477=CARTESIAN_POINT('Ctrl Pts',(-3.46198252886957,-9.78593684022037,-3.75));
#5478=CARTESIAN_POINT('Ctrl Pts',(-3.46198252886957,-9.78593684022037,12.75));
#5479=CARTESIAN_POINT('Ctrl Pts',(-3.41168916880891,-9.75022858813702,-3.75));
#5480=CARTESIAN_POINT('Ctrl Pts',(-3.41168916880891,-9.75022858813702,12.75));
#5481=CARTESIAN_POINT('Ctrl Pts',(-3.36192803839197,-9.7141195953304,-3.75));
#5482=CARTESIAN_POINT('Ctrl Pts',(-3.36192803839197,-9.7141195953304,12.75));
#5483=CARTESIAN_POINT('Ctrl Pts',(-3.31270665744062,-9.67761177523123,-3.75));
#5484=CARTESIAN_POINT('Ctrl Pts',(-3.31270665744062,-9.67761177523123,12.75));
#5485=CARTESIAN_POINT('Ctrl Pts',(-3.26403452382223,-9.64070633286081,-3.75));
#5486=CARTESIAN_POINT('Ctrl Pts',(-3.26403452382223,-9.64070633286081,12.75));
#5487=CARTESIAN_POINT('Ctrl Pts',(-3.2159238260067,-9.60340349406962,-3.75));
#5488=CARTESIAN_POINT('Ctrl Pts',(-3.2159238260067,-9.60340349406962,12.75));
#5489=CARTESIAN_POINT('Ctrl Pts',(-3.16838785383004,-9.56570313257491,-3.75));
#5490=CARTESIAN_POINT('Ctrl Pts',(-3.16838785383004,-9.56570313257491,12.75));
#5491=CARTESIAN_POINT('Ctrl Pts',(-3.121439393007,-9.52760540436562,-3.75));
#5492=CARTESIAN_POINT('Ctrl Pts',(-3.121439393007,-9.52760540436562,12.75));
#5493=CARTESIAN_POINT('Ctrl Pts',(-3.07508913212204,-9.4891113781729,-3.75));
#5494=CARTESIAN_POINT('Ctrl Pts',(-3.07508913212204,-9.4891113781729,12.75));
#5495=CARTESIAN_POINT('Ctrl Pts',(-3.02934403325601,-9.4502236812248,-3.75));
#5496=CARTESIAN_POINT('Ctrl Pts',(-3.02934403325601,-9.4502236812248,12.75));
#5497=CARTESIAN_POINT('Ctrl Pts',(-2.98420577513996,-9.4109471173216,-3.75));
#5498=CARTESIAN_POINT('Ctrl Pts',(-2.98420577513996,-9.4109471173216,12.75));
#5499=CARTESIAN_POINT('Ctrl Pts',(-2.9396747031485,-9.3712871143499,-3.75));
#5500=CARTESIAN_POINT('Ctrl Pts',(-2.9396747031485,-9.3712871143499,12.75));
#5501=CARTESIAN_POINT('Ctrl Pts',(-2.89575377593938,-9.33124817395868,-3.75));
#5502=CARTESIAN_POINT('Ctrl Pts',(-2.89575377593938,-9.33124817395868,12.75));
#5503=CARTESIAN_POINT('Ctrl Pts',(-2.8524523828002,-9.29083237315974,-3.75));
#5504=CARTESIAN_POINT('Ctrl Pts',(-2.8524523828002,-9.29083237315974,12.75));
#5505=CARTESIAN_POINT('Ctrl Pts',(-2.8097905150733,-9.2500377269296,-3.75));
#5506=CARTESIAN_POINT('Ctrl Pts',(-2.8097905150733,-9.2500377269296,12.75));
#5507=CARTESIAN_POINT('Ctrl Pts',(-2.76780196452137,-9.20885693589776,-3.75));
#5508=CARTESIAN_POINT('Ctrl Pts',(-2.76780196452137,-9.20885693589776,12.75));
#5509=CARTESIAN_POINT('Ctrl Pts',(-2.72652481622917,-9.16728115317076,-3.75));
#5510=CARTESIAN_POINT('Ctrl Pts',(-2.72652481622917,-9.16728115317076,12.75));
#5511=CARTESIAN_POINT('Ctrl Pts',(-2.68599232523134,-9.12530360007999,-3.75));
#5512=CARTESIAN_POINT('Ctrl Pts',(-2.68599232523134,-9.12530360007999,12.75));
#5513=CARTESIAN_POINT('Ctrl Pts',(-2.64622438896053,-9.08292294803309,-3.75));
#5514=CARTESIAN_POINT('Ctrl Pts',(-2.64622438896053,-9.08292294803309,12.75));
#5515=CARTESIAN_POINT('Ctrl Pts',(-2.6072169995188,-9.0401474973841,-3.75));
#5516=CARTESIAN_POINT('Ctrl Pts',(-2.6072169995188,-9.0401474973841,12.75));
#5517=CARTESIAN_POINT('Ctrl Pts',(-2.5689376774732,-8.99699699918147,-3.75));
#5518=CARTESIAN_POINT('Ctrl Pts',(-2.5689376774732,-8.99699699918147,12.75));
#5519=CARTESIAN_POINT('Ctrl Pts',(-2.53134978004338,-8.95349309713545,-3.75));
#5520=CARTESIAN_POINT('Ctrl Pts',(-2.53134978004338,-8.95349309713545,12.75));
#5521=CARTESIAN_POINT('Ctrl Pts',(-2.49443464151821,-8.90965062344541,-3.75));
#5522=CARTESIAN_POINT('Ctrl Pts',(-2.49443464151821,-8.90965062344541,12.75));
#5523=CARTESIAN_POINT('Ctrl Pts',(-2.45821141167119,-8.86546980570045,-3.75));
#5524=CARTESIAN_POINT('Ctrl Pts',(-2.45821141167119,-8.86546980570045,12.75));
#5525=CARTESIAN_POINT('Ctrl Pts',(-2.42276538248091,-8.82092512134555,-3.75));
#5526=CARTESIAN_POINT('Ctrl Pts',(-2.42276538248091,-8.82092512134555,12.75));
#5527=CARTESIAN_POINT('Ctrl Pts',(-2.38824857383289,-8.77596511266658,-3.75));
#5528=CARTESIAN_POINT('Ctrl Pts',(-2.38824857383289,-8.77596511266658,12.75));
#5529=CARTESIAN_POINT('Ctrl Pts',(-2.35482147675118,-8.73053548487858,-3.75));
#5530=CARTESIAN_POINT('Ctrl Pts',(-2.35482147675118,-8.73053548487858,12.75));
#5531=CARTESIAN_POINT('Ctrl Pts',(-2.32260171926006,-8.68459942442028,-3.75));
#5532=CARTESIAN_POINT('Ctrl Pts',(-2.32260171926006,-8.68459942442028,12.75));
#5533=CARTESIAN_POINT('Ctrl Pts',(-2.29162050823336,-8.63815494571075,-3.75));
#5534=CARTESIAN_POINT('Ctrl Pts',(-2.29162050823336,-8.63815494571075,12.75));
#5535=CARTESIAN_POINT('Ctrl Pts',(-2.26174990860572,-8.59126351952004,-3.75));
#5536=CARTESIAN_POINT('Ctrl Pts',(-2.26174990860572,-8.59126351952004,12.75));
#5537=CARTESIAN_POINT('Ctrl Pts',(-2.23274297834756,-8.54403497990068,-3.75));
#5538=CARTESIAN_POINT('Ctrl Pts',(-2.23274297834756,-8.54403497990068,12.75));
#5539=CARTESIAN_POINT('Ctrl Pts',(-2.20438215159744,-8.49657041043195,-3.75));
#5540=CARTESIAN_POINT('Ctrl Pts',(-2.20438215159744,-8.49657041043195,12.75));
#5541=CARTESIAN_POINT('Ctrl Pts',(-2.17660700812682,-8.44891314968814,-3.75));
#5542=CARTESIAN_POINT('Ctrl Pts',(-2.17660700812682,-8.44891314968814,12.75));
#5543=CARTESIAN_POINT('Ctrl Pts',(-2.1496314108288,-8.40100363162428,-3.75));
#5544=CARTESIAN_POINT('Ctrl Pts',(-2.1496314108288,-8.40100363162428,12.75));
#5545=CARTESIAN_POINT('Ctrl Pts',(-2.12411443763999,-8.35261410600662,-3.75));
#5546=CARTESIAN_POINT('Ctrl Pts',(-2.12411443763999,-8.35261410600662,12.75));
#5547=CARTESIAN_POINT('Ctrl Pts',(-2.10101049300139,-8.3034037182712,-3.75));
#5548=CARTESIAN_POINT('Ctrl Pts',(-2.10101049300139,-8.3034037182712,12.75));
#5549=CARTESIAN_POINT('Ctrl Pts',(-2.08524426770063,-8.26309465918435,-3.75));
#5550=CARTESIAN_POINT('Ctrl Pts',(-2.08524426770063,-8.26309465918435,12.75));
#5551=CARTESIAN_POINT('Ctrl Pts',(-2.07530073900945,-8.23220544002367,-3.75));
#5552=CARTESIAN_POINT('Ctrl Pts',(-2.07530073900945,-8.23220544002367,12.75));
#5553=CARTESIAN_POINT('Ctrl Pts',(-2.06955313972064,-8.21130388109186,-3.75));
#5554=CARTESIAN_POINT('Ctrl Pts',(-2.06955313972064,-8.21130388109186,12.75));
#5555=CARTESIAN_POINT('Ctrl Pts',(-2.06689970121501,-8.20077591276801,-3.75));
#5556=CARTESIAN_POINT('Ctrl Pts',(-2.06689970121501,-8.20077591276801,12.75));
#5557=CARTESIAN_POINT('',(-5.3791293750062,-10.7268339768519,-1.));
#5558=CARTESIAN_POINT('Ctrl Pts',(-5.37912937500618,-10.726833976852,-1.));
#5559=CARTESIAN_POINT('Ctrl Pts',(-5.36620715918271,-10.7225897134991,-1.));
#5560=CARTESIAN_POINT('Ctrl Pts',(-5.34039795525199,-10.714055870666,-1.));
#5561=CARTESIAN_POINT('Ctrl Pts',(-5.30178983253177,-10.7011191580639,-1.));
#5562=CARTESIAN_POINT('Ctrl Pts',(-5.25052377191006,-10.6835982206291,-1.));
#5563=CARTESIAN_POINT('Ctrl Pts',(-5.18679427410258,-10.661243291145,-1.));
#5564=CARTESIAN_POINT('Ctrl Pts',(-5.12341919820984,-10.638434168447,-1.));
#5565=CARTESIAN_POINT('Ctrl Pts',(-5.06040071098369,-10.6151706715837,-1.));
#5566=CARTESIAN_POINT('Ctrl Pts',(-4.99774193408265,-10.5914530920551,-1.));
#5567=CARTESIAN_POINT('Ctrl Pts',(-4.93544714999768,-10.5672824880187,-1.));
#5568=CARTESIAN_POINT('Ctrl Pts',(-4.87352158939686,-10.5426605691059,-1.));
#5569=CARTESIAN_POINT('Ctrl Pts',(-4.81197108362036,-10.5175894490106,-1.));
#5570=CARTESIAN_POINT('Ctrl Pts',(-4.7508017470924,-10.4920714379865,-1.));
#5571=CARTESIAN_POINT('Ctrl Pts',(-4.69001967404875,-10.4661088391609,-1.));
#5572=CARTESIAN_POINT('Ctrl Pts',(-4.62963055491846,-10.4397037052484,-1.));
#5573=CARTESIAN_POINT('Ctrl Pts',(-4.56963961142454,-10.4128577818052,-1.));
#5574=CARTESIAN_POINT('Ctrl Pts',(-4.5100518320603,-10.3855726289458,-1.));
#5575=CARTESIAN_POINT('Ctrl Pts',(-4.45087212698486,-10.3578496987941,-1.));
#5576=CARTESIAN_POINT('Ctrl Pts',(-4.39210550098945,-10.3296904287044,-1.));
#5577=CARTESIAN_POINT('Ctrl Pts',(-4.33375724408484,-10.3010963438997,-1.));
#5578=CARTESIAN_POINT('Ctrl Pts',(-4.27583301771354,-10.272069116189,-1.));
#5579=CARTESIAN_POINT('Ctrl Pts',(-4.21833871177567,-10.2426105188232,-1.));
#5580=CARTESIAN_POINT('Ctrl Pts',(-4.16128034451963,-10.2127224064663,-1.));
#5581=CARTESIAN_POINT('Ctrl Pts',(-4.10466394929486,-10.1824066879509,-1.));
#5582=CARTESIAN_POINT('Ctrl Pts',(-4.04849544744087,-10.1516653064199,-1.));
#5583=CARTESIAN_POINT('Ctrl Pts',(-3.99278057289047,-10.1205002164952,-1.));
#5584=CARTESIAN_POINT('Ctrl Pts',(-3.93752506012707,-10.0889133486827,-1.));
#5585=CARTESIAN_POINT('Ctrl Pts',(-3.88273479532263,-10.056906577166,-1.));
#5586=CARTESIAN_POINT('Ctrl Pts',(-3.82841597408715,-10.0244816905709,-1.));
#5587=CARTESIAN_POINT('Ctrl Pts',(-3.77457526401005,-9.99164036147395,-1.));
#5588=CARTESIAN_POINT('Ctrl Pts',(-3.72121993173637,-9.95838412799172,-1.));
#5589=CARTESIAN_POINT('Ctrl Pts',(-3.66835753420626,-9.92471449880882,-1.));
#5590=CARTESIAN_POINT('Ctrl Pts',(-3.61599563628969,-9.89063305253546,-1.));
#5591=CARTESIAN_POINT('Ctrl Pts',(-3.56414151726151,-9.8561415413778,-1.));
#5592=CARTESIAN_POINT('Ctrl Pts',(-3.51280187273296,-9.8212419982557,-1.));
#5593=CARTESIAN_POINT('Ctrl Pts',(-3.46198252886957,-9.78593684022037,-1.));
#5594=CARTESIAN_POINT('Ctrl Pts',(-3.41168916880891,-9.75022858813702,-1.));
#5595=CARTESIAN_POINT('Ctrl Pts',(-3.36192803839197,-9.7141195953304,-1.));
#5596=CARTESIAN_POINT('Ctrl Pts',(-3.31270665744062,-9.67761177523123,-1.));
#5597=CARTESIAN_POINT('Ctrl Pts',(-3.26403452382223,-9.64070633286081,-1.));
#5598=CARTESIAN_POINT('Ctrl Pts',(-3.2159238260067,-9.60340349406962,-1.));
#5599=CARTESIAN_POINT('Ctrl Pts',(-3.16838785383004,-9.56570313257491,-1.));
#5600=CARTESIAN_POINT('Ctrl Pts',(-3.121439393007,-9.52760540436562,-1.));
#5601=CARTESIAN_POINT('Ctrl Pts',(-3.07508913212204,-9.4891113781729,-1.));
#5602=CARTESIAN_POINT('Ctrl Pts',(-3.02934403325601,-9.4502236812248,-1.));
#5603=CARTESIAN_POINT('Ctrl Pts',(-2.98420577513996,-9.4109471173216,-1.));
#5604=CARTESIAN_POINT('Ctrl Pts',(-2.9396747031485,-9.3712871143499,-1.));
#5605=CARTESIAN_POINT('Ctrl Pts',(-2.89575377593938,-9.33124817395868,-1.));
#5606=CARTESIAN_POINT('Ctrl Pts',(-2.8524523828002,-9.29083237315974,-1.));
#5607=CARTESIAN_POINT('Ctrl Pts',(-2.8097905150733,-9.2500377269296,-1.));
#5608=CARTESIAN_POINT('Ctrl Pts',(-2.76780196452137,-9.20885693589776,-1.));
#5609=CARTESIAN_POINT('Ctrl Pts',(-2.72652481622917,-9.16728115317076,-1.));
#5610=CARTESIAN_POINT('Ctrl Pts',(-2.68599232523134,-9.12530360007999,-1.));
#5611=CARTESIAN_POINT('Ctrl Pts',(-2.64622438896053,-9.08292294803309,-1.));
#5612=CARTESIAN_POINT('Ctrl Pts',(-2.6072169995188,-9.0401474973841,-1.));
#5613=CARTESIAN_POINT('Ctrl Pts',(-2.5689376774732,-8.99699699918147,-1.));
#5614=CARTESIAN_POINT('Ctrl Pts',(-2.53134978004338,-8.95349309713545,-1.));
#5615=CARTESIAN_POINT('Ctrl Pts',(-2.49443464151821,-8.90965062344541,-1.));
#5616=CARTESIAN_POINT('Ctrl Pts',(-2.45821141167119,-8.86546980570045,-1.));
#5617=CARTESIAN_POINT('Ctrl Pts',(-2.42276538248091,-8.82092512134555,-1.));
#5618=CARTESIAN_POINT('Ctrl Pts',(-2.38824857383289,-8.77596511266658,-1.));
#5619=CARTESIAN_POINT('Ctrl Pts',(-2.35482147675118,-8.73053548487858,-1.));
#5620=CARTESIAN_POINT('Ctrl Pts',(-2.32260171926006,-8.68459942442028,-1.));
#5621=CARTESIAN_POINT('Ctrl Pts',(-2.29162050823336,-8.63815494571075,-1.));
#5622=CARTESIAN_POINT('Ctrl Pts',(-2.26174990860572,-8.59126351952004,-1.));
#5623=CARTESIAN_POINT('Ctrl Pts',(-2.23274297834756,-8.54403497990068,-1.));
#5624=CARTESIAN_POINT('Ctrl Pts',(-2.20438215159744,-8.49657041043195,-1.));
#5625=CARTESIAN_POINT('Ctrl Pts',(-2.17660700812682,-8.44891314968814,-1.));
#5626=CARTESIAN_POINT('Ctrl Pts',(-2.1496314108288,-8.40100363162428,-1.));
#5627=CARTESIAN_POINT('Ctrl Pts',(-2.12411443763999,-8.35261410600662,-1.));
#5628=CARTESIAN_POINT('Ctrl Pts',(-2.10101049300139,-8.3034037182712,-1.));
#5629=CARTESIAN_POINT('Ctrl Pts',(-2.08524426770063,-8.26309465918435,-1.));
#5630=CARTESIAN_POINT('Ctrl Pts',(-2.07530073900945,-8.23220544002367,-1.));
#5631=CARTESIAN_POINT('Ctrl Pts',(-2.06955313972064,-8.21130388109186,-1.));
#5632=CARTESIAN_POINT('Ctrl Pts',(-2.06689970121501,-8.20077591276801,-1.));
#5633=CARTESIAN_POINT('',(-5.3791293750062,-10.7268339768519,6.));
#5634=CARTESIAN_POINT('Ctrl Pts',(-5.37912937500618,-10.726833976852,6.));
#5635=CARTESIAN_POINT('Ctrl Pts',(-5.36620715918271,-10.7225897134991,6.));
#5636=CARTESIAN_POINT('Ctrl Pts',(-5.34039795525199,-10.714055870666,6.));
#5637=CARTESIAN_POINT('Ctrl Pts',(-5.30178983253177,-10.7011191580639,6.));
#5638=CARTESIAN_POINT('Ctrl Pts',(-5.25052377191006,-10.6835982206291,6.));
#5639=CARTESIAN_POINT('Ctrl Pts',(-5.18679427410258,-10.661243291145,6.));
#5640=CARTESIAN_POINT('Ctrl Pts',(-5.12341919820984,-10.638434168447,6.));
#5641=CARTESIAN_POINT('Ctrl Pts',(-5.06040071098369,-10.6151706715837,6.));
#5642=CARTESIAN_POINT('Ctrl Pts',(-4.99774193408265,-10.5914530920551,6.));
#5643=CARTESIAN_POINT('Ctrl Pts',(-4.93544714999768,-10.5672824880187,6.));
#5644=CARTESIAN_POINT('Ctrl Pts',(-4.87352158939686,-10.5426605691059,6.));
#5645=CARTESIAN_POINT('Ctrl Pts',(-4.81197108362036,-10.5175894490106,6.));
#5646=CARTESIAN_POINT('Ctrl Pts',(-4.7508017470924,-10.4920714379865,6.));
#5647=CARTESIAN_POINT('Ctrl Pts',(-4.69001967404875,-10.4661088391609,6.));
#5648=CARTESIAN_POINT('Ctrl Pts',(-4.62963055491846,-10.4397037052484,6.));
#5649=CARTESIAN_POINT('Ctrl Pts',(-4.56963961142454,-10.4128577818052,6.));
#5650=CARTESIAN_POINT('Ctrl Pts',(-4.5100518320603,-10.3855726289458,6.));
#5651=CARTESIAN_POINT('Ctrl Pts',(-4.45087212698486,-10.3578496987941,6.));
#5652=CARTESIAN_POINT('Ctrl Pts',(-4.39210550098945,-10.3296904287044,6.));
#5653=CARTESIAN_POINT('Ctrl Pts',(-4.33375724408484,-10.3010963438997,6.));
#5654=CARTESIAN_POINT('Ctrl Pts',(-4.27583301771354,-10.272069116189,6.));
#5655=CARTESIAN_POINT('Ctrl Pts',(-4.21833871177567,-10.2426105188232,6.));
#5656=CARTESIAN_POINT('Ctrl Pts',(-4.16128034451963,-10.2127224064663,6.));
#5657=CARTESIAN_POINT('Ctrl Pts',(-4.10466394929486,-10.1824066879509,6.));
#5658=CARTESIAN_POINT('Ctrl Pts',(-4.04849544744087,-10.1516653064199,6.));
#5659=CARTESIAN_POINT('Ctrl Pts',(-3.99278057289047,-10.1205002164952,6.));
#5660=CARTESIAN_POINT('Ctrl Pts',(-3.93752506012707,-10.0889133486827,6.));
#5661=CARTESIAN_POINT('Ctrl Pts',(-3.88273479532263,-10.056906577166,6.));
#5662=CARTESIAN_POINT('Ctrl Pts',(-3.82841597408715,-10.0244816905709,6.));
#5663=CARTESIAN_POINT('Ctrl Pts',(-3.77457526401005,-9.99164036147395,6.));
#5664=CARTESIAN_POINT('Ctrl Pts',(-3.72121993173637,-9.95838412799172,6.));
#5665=CARTESIAN_POINT('Ctrl Pts',(-3.66835753420626,-9.92471449880882,6.));
#5666=CARTESIAN_POINT('Ctrl Pts',(-3.61599563628969,-9.89063305253546,6.));
#5667=CARTESIAN_POINT('Ctrl Pts',(-3.56414151726151,-9.8561415413778,6.));
#5668=CARTESIAN_POINT('Ctrl Pts',(-3.51280187273296,-9.8212419982557,6.));
#5669=CARTESIAN_POINT('Ctrl Pts',(-3.46198252886957,-9.78593684022037,6.));
#5670=CARTESIAN_POINT('Ctrl Pts',(-3.41168916880891,-9.75022858813702,6.));
#5671=CARTESIAN_POINT('Ctrl Pts',(-3.36192803839197,-9.7141195953304,6.));
#5672=CARTESIAN_POINT('Ctrl Pts',(-3.31270665744062,-9.67761177523123,6.));
#5673=CARTESIAN_POINT('Ctrl Pts',(-3.26403452382223,-9.64070633286081,6.));
#5674=CARTESIAN_POINT('Ctrl Pts',(-3.2159238260067,-9.60340349406962,6.));
#5675=CARTESIAN_POINT('Ctrl Pts',(-3.16838785383004,-9.56570313257491,6.));
#5676=CARTESIAN_POINT('Ctrl Pts',(-3.121439393007,-9.52760540436562,6.));
#5677=CARTESIAN_POINT('Ctrl Pts',(-3.07508913212204,-9.4891113781729,6.));
#5678=CARTESIAN_POINT('Ctrl Pts',(-3.02934403325601,-9.4502236812248,6.));
#5679=CARTESIAN_POINT('Ctrl Pts',(-2.98420577513996,-9.4109471173216,6.));
#5680=CARTESIAN_POINT('Ctrl Pts',(-2.9396747031485,-9.3712871143499,6.));
#5681=CARTESIAN_POINT('Ctrl Pts',(-2.89575377593938,-9.33124817395868,6.));
#5682=CARTESIAN_POINT('Ctrl Pts',(-2.8524523828002,-9.29083237315974,6.));
#5683=CARTESIAN_POINT('Ctrl Pts',(-2.8097905150733,-9.2500377269296,6.));
#5684=CARTESIAN_POINT('Ctrl Pts',(-2.76780196452137,-9.20885693589776,6.));
#5685=CARTESIAN_POINT('Ctrl Pts',(-2.72652481622917,-9.16728115317076,6.));
#5686=CARTESIAN_POINT('Ctrl Pts',(-2.68599232523134,-9.12530360007999,6.));
#5687=CARTESIAN_POINT('Ctrl Pts',(-2.64622438896053,-9.08292294803309,6.));
#5688=CARTESIAN_POINT('Ctrl Pts',(-2.6072169995188,-9.0401474973841,6.));
#5689=CARTESIAN_POINT('Ctrl Pts',(-2.5689376774732,-8.99699699918147,6.));
#5690=CARTESIAN_POINT('Ctrl Pts',(-2.53134978004338,-8.95349309713545,6.));
#5691=CARTESIAN_POINT('Ctrl Pts',(-2.49443464151821,-8.90965062344541,6.));
#5692=CARTESIAN_POINT('Ctrl Pts',(-2.45821141167119,-8.86546980570045,6.));
#5693=CARTESIAN_POINT('Ctrl Pts',(-2.42276538248091,-8.82092512134555,6.));
#5694=CARTESIAN_POINT('Ctrl Pts',(-2.38824857383289,-8.77596511266658,6.));
#5695=CARTESIAN_POINT('Ctrl Pts',(-2.35482147675118,-8.73053548487858,6.));
#5696=CARTESIAN_POINT('Ctrl Pts',(-2.32260171926006,-8.68459942442028,6.));
#5697=CARTESIAN_POINT('Ctrl Pts',(-2.29162050823336,-8.63815494571075,6.));
#5698=CARTESIAN_POINT('Ctrl Pts',(-2.26174990860572,-8.59126351952004,6.));
#5699=CARTESIAN_POINT('Ctrl Pts',(-2.23274297834756,-8.54403497990068,6.));
#5700=CARTESIAN_POINT('Ctrl Pts',(-2.20438215159744,-8.49657041043195,6.));
#5701=CARTESIAN_POINT('Ctrl Pts',(-2.17660700812682,-8.44891314968814,6.));
#5702=CARTESIAN_POINT('Ctrl Pts',(-2.1496314108288,-8.40100363162428,6.));
#5703=CARTESIAN_POINT('Ctrl Pts',(-2.12411443763999,-8.35261410600662,6.));
#5704=CARTESIAN_POINT('Ctrl Pts',(-2.10101049300139,-8.3034037182712,6.));
#5705=CARTESIAN_POINT('Ctrl Pts',(-2.08524426770063,-8.26309465918435,6.));
#5706=CARTESIAN_POINT('Ctrl Pts',(-2.07530073900945,-8.23220544002367,6.));
#5707=CARTESIAN_POINT('Ctrl Pts',(-2.06955313972064,-8.21130388109186,6.));
#5708=CARTESIAN_POINT('Ctrl Pts',(-2.06689970121501,-8.20077591276801,6.));
#5709=CARTESIAN_POINT('',(-5.3791293750062,-10.7268339768519,0.));
#5710=CARTESIAN_POINT('Origin',(-1.99840144432528E-13,-3.46133283549041E-13,
0.));
#5711=CARTESIAN_POINT('',(-6.60014603862878,-10.0218796774244,-1.));
#5712=CARTESIAN_POINT('Origin',(-1.99840144432528E-13,-3.46133283549041E-13,
-1.));
#5713=CARTESIAN_POINT('',(-6.60014603862878,-10.0218796774244,6.));
#5714=CARTESIAN_POINT('Origin',(-1.99840144432528E-13,-3.46133283549041E-13,
6.));
#5715=CARTESIAN_POINT('',(-6.60014603862878,-10.0218796774244,0.));
#5716=CARTESIAN_POINT('Ctrl Pts',(-6.06863042059311,-5.89037560471066,-3.75));
#5717=CARTESIAN_POINT('Ctrl Pts',(-6.06863042059311,-5.89037560471066,12.75));
#5718=CARTESIAN_POINT('Ctrl Pts',(-6.076421189359,-5.89793753402584,-3.75));
#5719=CARTESIAN_POINT('Ctrl Pts',(-6.076421189359,-5.89793753402584,12.75));
#5720=CARTESIAN_POINT('Ctrl Pts',(-6.09164867072824,-5.91336588048663,-3.75));
#5721=CARTESIAN_POINT('Ctrl Pts',(-6.09164867072824,-5.91336588048663,12.75));
#5722=CARTESIAN_POINT('Ctrl Pts',(-6.11342775487885,-5.93742183851679,-3.75));
#5723=CARTESIAN_POINT('Ctrl Pts',(-6.11342775487885,-5.93742183851679,12.75));
#5724=CARTESIAN_POINT('Ctrl Pts',(-6.14045331140034,-5.97123031969246,-3.75));
#5725=CARTESIAN_POINT('Ctrl Pts',(-6.14045331140034,-5.97123031969246,12.75));
#5726=CARTESIAN_POINT('Ctrl Pts',(-6.17151878498999,-6.01584411654483,-3.75));
#5727=CARTESIAN_POINT('Ctrl Pts',(-6.17151878498999,-6.01584411654483,12.75));
#5728=CARTESIAN_POINT('Ctrl Pts',(-6.20066685685755,-6.06213722636286,-3.75));
#5729=CARTESIAN_POINT('Ctrl Pts',(-6.20066685685755,-6.06213722636286,12.75));
#5730=CARTESIAN_POINT('Ctrl Pts',(-6.22866991793492,-6.10945353793713,-3.75));
#5731=CARTESIAN_POINT('Ctrl Pts',(-6.22866991793492,-6.10945353793713,12.75));
#5732=CARTESIAN_POINT('Ctrl Pts',(-6.25605474467853,-6.15733614814835,-3.75));
#5733=CARTESIAN_POINT('Ctrl Pts',(-6.25605474467853,-6.15733614814835,12.75));
#5734=CARTESIAN_POINT('Ctrl Pts',(-6.28297985424308,-6.20562962932064,-3.75));
#5735=CARTESIAN_POINT('Ctrl Pts',(-6.28297985424308,-6.20562962932064,12.75));
#5736=CARTESIAN_POINT('Ctrl Pts',(-6.30937750420801,-6.2543646376197,-3.75));
#5737=CARTESIAN_POINT('Ctrl Pts',(-6.30937750420801,-6.2543646376197,12.75));
#5738=CARTESIAN_POINT('Ctrl Pts',(-6.33505137069502,-6.30367904881886,-3.75));
#5739=CARTESIAN_POINT('Ctrl Pts',(-6.33505137069502,-6.30367904881886,12.75));
#5740=CARTESIAN_POINT('Ctrl Pts',(-6.35978286360965,-6.35373180396276,-3.75));
#5741=CARTESIAN_POINT('Ctrl Pts',(-6.35978286360965,-6.35373180396276,12.75));
#5742=CARTESIAN_POINT('Ctrl Pts',(-6.38345478017076,-6.40460296268299,-3.75));
#5743=CARTESIAN_POINT('Ctrl Pts',(-6.38345478017076,-6.40460296268299,12.75));
#5744=CARTESIAN_POINT('Ctrl Pts',(-6.40608444337878,-6.45626649182452,-3.75));
#5745=CARTESIAN_POINT('Ctrl Pts',(-6.40608444337878,-6.45626649182452,12.75));
#5746=CARTESIAN_POINT('Ctrl Pts',(-6.42776254872514,-6.50863892931076,-3.75));
#5747=CARTESIAN_POINT('Ctrl Pts',(-6.42776254872514,-6.50863892931076,12.75));
#5748=CARTESIAN_POINT('Ctrl Pts',(-6.44861636238489,-6.56160843323027,-3.75));
#5749=CARTESIAN_POINT('Ctrl Pts',(-6.44861636238489,-6.56160843323027,12.75));
#5750=CARTESIAN_POINT('Ctrl Pts',(-6.46876645798849,-6.6150690793574,-3.75));
#5751=CARTESIAN_POINT('Ctrl Pts',(-6.46876645798849,-6.6150690793574,12.75));
#5752=CARTESIAN_POINT('Ctrl Pts',(-6.48827758470623,-6.66895976394943,-3.75));
#5753=CARTESIAN_POINT('Ctrl Pts',(-6.48827758470623,-6.66895976394943,12.75));
#5754=CARTESIAN_POINT('Ctrl Pts',(-6.50715912032692,-6.72326378902151,-3.75));
#5755=CARTESIAN_POINT('Ctrl Pts',(-6.50715912032692,-6.72326378902151,12.75));
#5756=CARTESIAN_POINT('Ctrl Pts',(-6.52538888693356,-6.77798990345396,-3.75));
#5757=CARTESIAN_POINT('Ctrl Pts',(-6.52538888693356,-6.77798990345396,12.75));
#5758=CARTESIAN_POINT('Ctrl Pts',(-6.54292981913304,-6.83315901897031,-3.75));
#5759=CARTESIAN_POINT('Ctrl Pts',(-6.54292981913304,-6.83315901897031,12.75));
#5760=CARTESIAN_POINT('Ctrl Pts',(-6.5597485722992,-6.88878938806037,-3.75));
#5761=CARTESIAN_POINT('Ctrl Pts',(-6.5597485722992,-6.88878938806037,12.75));
#5762=CARTESIAN_POINT('Ctrl Pts',(-6.57583595416561,-6.94488033148853,-3.75));
#5763=CARTESIAN_POINT('Ctrl Pts',(-6.57583595416561,-6.94488033148853,12.75));
#5764=CARTESIAN_POINT('Ctrl Pts',(-6.59120306404331,-7.00141528186886,-3.75));
#5765=CARTESIAN_POINT('Ctrl Pts',(-6.59120306404331,-7.00141528186886,12.75));
#5766=CARTESIAN_POINT('Ctrl Pts',(-6.60587239994886,-7.05836882883083,-3.75));
#5767=CARTESIAN_POINT('Ctrl Pts',(-6.60587239994886,-7.05836882883083,12.75));
#5768=CARTESIAN_POINT('Ctrl Pts',(-6.61987066605911,-7.11571241317029,-3.75));
#5769=CARTESIAN_POINT('Ctrl Pts',(-6.61987066605911,-7.11571241317029,12.75));
#5770=CARTESIAN_POINT('Ctrl Pts',(-6.63322107969569,-7.17342042004755,-3.75));
#5771=CARTESIAN_POINT('Ctrl Pts',(-6.63322107969569,-7.17342042004755,12.75));
#5772=CARTESIAN_POINT('Ctrl Pts',(-6.64593535561053,-7.23147652896402,-3.75));
#5773=CARTESIAN_POINT('Ctrl Pts',(-6.64593535561053,-7.23147652896402,12.75));
#5774=CARTESIAN_POINT('Ctrl Pts',(-6.65801638970246,-7.28987157005223,-3.75));
#5775=CARTESIAN_POINT('Ctrl Pts',(-6.65801638970246,-7.28987157005223,12.75));
#5776=CARTESIAN_POINT('Ctrl Pts',(-6.66946176275798,-7.34860073021491,-3.75));
#5777=CARTESIAN_POINT('Ctrl Pts',(-6.66946176275798,-7.34860073021491,12.75));
#5778=CARTESIAN_POINT('Ctrl Pts',(-6.68026694677668,-7.40766099640557,-3.75));
#5779=CARTESIAN_POINT('Ctrl Pts',(-6.68026694677668,-7.40766099640557,12.75));
#5780=CARTESIAN_POINT('Ctrl Pts',(-6.69042862091104,-7.46704851290034,-3.75));
#5781=CARTESIAN_POINT('Ctrl Pts',(-6.69042862091104,-7.46704851290034,12.75));
#5782=CARTESIAN_POINT('Ctrl Pts',(-6.69994799095524,-7.52675593674632,-3.75));
#5783=CARTESIAN_POINT('Ctrl Pts',(-6.69994799095524,-7.52675593674632,12.75));
#5784=CARTESIAN_POINT('Ctrl Pts',(-6.70882947565318,-7.58677347699225,-3.75));
#5785=CARTESIAN_POINT('Ctrl Pts',(-6.70882947565318,-7.58677347699225,12.75));
#5786=CARTESIAN_POINT('Ctrl Pts',(-6.71707933277187,-7.64708998288989,-3.75));
#5787=CARTESIAN_POINT('Ctrl Pts',(-6.71707933277187,-7.64708998288989,12.75));
#5788=CARTESIAN_POINT('Ctrl Pts',(-6.72470431659336,-7.70769400824502,-3.75));
#5789=CARTESIAN_POINT('Ctrl Pts',(-6.72470431659336,-7.70769400824502,12.75));
#5790=CARTESIAN_POINT('Ctrl Pts',(-6.73171032576036,-7.76857488460783,-3.75));
#5791=CARTESIAN_POINT('Ctrl Pts',(-6.73171032576036,-7.76857488460783,12.75));
#5792=CARTESIAN_POINT('Ctrl Pts',(-6.73810106562749,-7.82972378407324,-3.75));
#5793=CARTESIAN_POINT('Ctrl Pts',(-6.73810106562749,-7.82972378407324,12.75));
#5794=CARTESIAN_POINT('Ctrl Pts',(-6.74387863902608,-7.89113323756912,-3.75));
#5795=CARTESIAN_POINT('Ctrl Pts',(-6.74387863902608,-7.89113323756912,12.75));
#5796=CARTESIAN_POINT('Ctrl Pts',(-6.74904413083761,-7.95279665937613,-3.75));
#5797=CARTESIAN_POINT('Ctrl Pts',(-6.74904413083761,-7.95279665937613,12.75));
#5798=CARTESIAN_POINT('Ctrl Pts',(-6.75359819949755,-8.01470786732018,-3.75));
#5799=CARTESIAN_POINT('Ctrl Pts',(-6.75359819949755,-8.01470786732018,12.75));
#5800=CARTESIAN_POINT('Ctrl Pts',(-6.7575416648609,-8.07686060726827,-3.75));
#5801=CARTESIAN_POINT('Ctrl Pts',(-6.7575416648609,-8.07686060726827,12.75));
#5802=CARTESIAN_POINT('Ctrl Pts',(-6.76087611417306,-8.13924806419107,-3.75));
#5803=CARTESIAN_POINT('Ctrl Pts',(-6.76087611417306,-8.13924806419107,12.75));
#5804=CARTESIAN_POINT('Ctrl Pts',(-6.7636036696164,-8.20186305794854,-3.75));
#5805=CARTESIAN_POINT('Ctrl Pts',(-6.7636036696164,-8.20186305794854,12.75));
#5806=CARTESIAN_POINT('Ctrl Pts',(-6.76572674650935,-8.26469824786602,-3.75));
#5807=CARTESIAN_POINT('Ctrl Pts',(-6.76572674650935,-8.26469824786602,12.75));
#5808=CARTESIAN_POINT('Ctrl Pts',(-6.76724781676282,-8.32774633509908,-3.75));
#5809=CARTESIAN_POINT('Ctrl Pts',(-6.76724781676282,-8.32774633509908,12.75));
#5810=CARTESIAN_POINT('Ctrl Pts',(-6.76816918165128,-8.39100025749018,-3.75));
#5811=CARTESIAN_POINT('Ctrl Pts',(-6.76816918165128,-8.39100025749018,12.75));
#5812=CARTESIAN_POINT('Ctrl Pts',(-6.76849272647566,-8.45445340444926,-3.75));
#5813=CARTESIAN_POINT('Ctrl Pts',(-6.76849272647566,-8.45445340444926,12.75));
#5814=CARTESIAN_POINT('Ctrl Pts',(-6.76822000004555,-8.51809951610773,-3.75));
#5815=CARTESIAN_POINT('Ctrl Pts',(-6.76822000004555,-8.51809951610773,12.75));
#5816=CARTESIAN_POINT('Ctrl Pts',(-6.76735232235635,-8.58193255779939,-3.75));
#5817=CARTESIAN_POINT('Ctrl Pts',(-6.76735232235635,-8.58193255779939,12.75));
#5818=CARTESIAN_POINT('Ctrl Pts',(-6.76589088878266,-8.64594659806298,-3.75));
#5819=CARTESIAN_POINT('Ctrl Pts',(-6.76589088878266,-8.64594659806298,12.75));
#5820=CARTESIAN_POINT('Ctrl Pts',(-6.76383687353853,-8.71013569385599,-3.75));
#5821=CARTESIAN_POINT('Ctrl Pts',(-6.76383687353853,-8.71013569385599,12.75));
#5822=CARTESIAN_POINT('Ctrl Pts',(-6.76119155448275,-8.77449374557664,-3.75));
#5823=CARTESIAN_POINT('Ctrl Pts',(-6.76119155448275,-8.77449374557664,12.75));
#5824=CARTESIAN_POINT('Ctrl Pts',(-6.7579562951925,-8.8390145737747,-3.75));
#5825=CARTESIAN_POINT('Ctrl Pts',(-6.7579562951925,-8.8390145737747,12.75));
#5826=CARTESIAN_POINT('Ctrl Pts',(-6.75413249860576,-8.90369203916217,-3.75));
#5827=CARTESIAN_POINT('Ctrl Pts',(-6.75413249860576,-8.90369203916217,12.75));
#5828=CARTESIAN_POINT('Ctrl Pts',(-6.7497215739923,-8.96852015431046,-3.75));
#5829=CARTESIAN_POINT('Ctrl Pts',(-6.7497215739923,-8.96852015431046,12.75));
#5830=CARTESIAN_POINT('Ctrl Pts',(-6.74472490424423,-9.03349318036198,-3.75));
#5831=CARTESIAN_POINT('Ctrl Pts',(-6.74472490424423,-9.03349318036198,12.75));
#5832=CARTESIAN_POINT('Ctrl Pts',(-6.73914381348524,-9.09860577342165,-3.75));
#5833=CARTESIAN_POINT('Ctrl Pts',(-6.73914381348524,-9.09860577342165,12.75));
#5834=CARTESIAN_POINT('Ctrl Pts',(-6.73297955932548,-9.16385288053588,-3.75));
#5835=CARTESIAN_POINT('Ctrl Pts',(-6.73297955932548,-9.16385288053588,12.75));
#5836=CARTESIAN_POINT('Ctrl Pts',(-6.72623333926846,-9.22922952332025,-3.75));
#5837=CARTESIAN_POINT('Ctrl Pts',(-6.72623333926846,-9.22922952332025,12.75));
#5838=CARTESIAN_POINT('Ctrl Pts',(-6.71890629646187,-9.2947306015555,-3.75));
#5839=CARTESIAN_POINT('Ctrl Pts',(-6.71890629646187,-9.2947306015555,12.75));
#5840=CARTESIAN_POINT('Ctrl Pts',(-6.71099953007124,-9.36035072031876,-3.75));
#5841=CARTESIAN_POINT('Ctrl Pts',(-6.71099953007124,-9.36035072031876,12.75));
#5842=CARTESIAN_POINT('Ctrl Pts',(-6.7025141076082,-9.42608392519666,-3.75));
#5843=CARTESIAN_POINT('Ctrl Pts',(-6.7025141076082,-9.42608392519666,12.75));
#5844=CARTESIAN_POINT('Ctrl Pts',(-6.69345108162377,-9.49192378686253,-3.75));
#5845=CARTESIAN_POINT('Ctrl Pts',(-6.69345108162377,-9.49192378686253,12.75));
#5846=CARTESIAN_POINT('Ctrl Pts',(-6.68381150859183,-9.55786385494286,-3.75));
#5847=CARTESIAN_POINT('Ctrl Pts',(-6.68381150859183,-9.55786385494286,12.75));
#5848=CARTESIAN_POINT('Ctrl Pts',(-6.67359647366962,-9.62389802250187,-3.75));
#5849=CARTESIAN_POINT('Ctrl Pts',(-6.67359647366962,-9.62389802250187,12.75));
#5850=CARTESIAN_POINT('Ctrl Pts',(-6.6628071116072,-9.69002090483257,-3.75));
#5851=CARTESIAN_POINT('Ctrl Pts',(-6.6628071116072,-9.69002090483257,12.75));
#5852=CARTESIAN_POINT('Ctrl Pts',(-6.65144464725859,-9.75622826411013,-3.75));
#5853=CARTESIAN_POINT('Ctrl Pts',(-6.65144464725859,-9.75622826411013,12.75));
#5854=CARTESIAN_POINT('Ctrl Pts',(-6.63951038900667,-9.82251725114898,-3.75));
#5855=CARTESIAN_POINT('Ctrl Pts',(-6.63951038900667,-9.82251725114898,12.75));
#5856=CARTESIAN_POINT('Ctrl Pts',(-6.62700557693596,-9.88888607996273,-3.75));
#5857=CARTESIAN_POINT('Ctrl Pts',(-6.62700557693596,-9.88888607996273,12.75));
#5858=CARTESIAN_POINT('Ctrl Pts',(-6.61654612354184,-9.94204425953052,-3.75));
#5859=CARTESIAN_POINT('Ctrl Pts',(-6.61654612354184,-9.94204425953052,12.75));
#5860=CARTESIAN_POINT('Ctrl Pts',(-6.60844558393657,-9.98194823089968,-3.75));
#5861=CARTESIAN_POINT('Ctrl Pts',(-6.60844558393657,-9.98194823089968,12.75));
#5862=CARTESIAN_POINT('Ctrl Pts',(-6.60293150665659,-10.0085665785717,-3.75));
#5863=CARTESIAN_POINT('Ctrl Pts',(-6.60293150665659,-10.0085665785717,12.75));
#5864=CARTESIAN_POINT('Ctrl Pts',(-6.60014603862878,-10.0218796774244,-3.75));
#5865=CARTESIAN_POINT('Ctrl Pts',(-6.60014603862878,-10.0218796774244,12.75));
#5866=CARTESIAN_POINT('Ctrl Pts',(-6.06863042059311,-5.89037560471066,-1.));
#5867=CARTESIAN_POINT('Ctrl Pts',(-6.076421189359,-5.89793753402584,-1.));
#5868=CARTESIAN_POINT('Ctrl Pts',(-6.09164867072824,-5.91336588048663,-1.));
#5869=CARTESIAN_POINT('Ctrl Pts',(-6.11342775487885,-5.93742183851679,-1.));
#5870=CARTESIAN_POINT('Ctrl Pts',(-6.14045331140034,-5.97123031969246,-1.));
#5871=CARTESIAN_POINT('Ctrl Pts',(-6.17151878498999,-6.01584411654483,-1.));
#5872=CARTESIAN_POINT('Ctrl Pts',(-6.20066685685755,-6.06213722636286,-1.));
#5873=CARTESIAN_POINT('Ctrl Pts',(-6.22866991793492,-6.10945353793713,-1.));
#5874=CARTESIAN_POINT('Ctrl Pts',(-6.25605474467853,-6.15733614814835,-1.));
#5875=CARTESIAN_POINT('Ctrl Pts',(-6.28297985424308,-6.20562962932064,-1.));
#5876=CARTESIAN_POINT('Ctrl Pts',(-6.30937750420801,-6.2543646376197,-1.));
#5877=CARTESIAN_POINT('Ctrl Pts',(-6.33505137069502,-6.30367904881886,-1.));
#5878=CARTESIAN_POINT('Ctrl Pts',(-6.35978286360965,-6.35373180396276,-1.));
#5879=CARTESIAN_POINT('Ctrl Pts',(-6.38345478017076,-6.40460296268299,-1.));
#5880=CARTESIAN_POINT('Ctrl Pts',(-6.40608444337878,-6.45626649182452,-1.));
#5881=CARTESIAN_POINT('Ctrl Pts',(-6.42776254872514,-6.50863892931076,-1.));
#5882=CARTESIAN_POINT('Ctrl Pts',(-6.44861636238489,-6.56160843323027,-1.));
#5883=CARTESIAN_POINT('Ctrl Pts',(-6.46876645798849,-6.6150690793574,-1.));
#5884=CARTESIAN_POINT('Ctrl Pts',(-6.48827758470623,-6.66895976394943,-1.));
#5885=CARTESIAN_POINT('Ctrl Pts',(-6.50715912032692,-6.72326378902151,-1.));
#5886=CARTESIAN_POINT('Ctrl Pts',(-6.52538888693356,-6.77798990345396,-1.));
#5887=CARTESIAN_POINT('Ctrl Pts',(-6.54292981913304,-6.83315901897031,-1.));
#5888=CARTESIAN_POINT('Ctrl Pts',(-6.5597485722992,-6.88878938806037,-1.));
#5889=CARTESIAN_POINT('Ctrl Pts',(-6.57583595416561,-6.94488033148853,-1.));
#5890=CARTESIAN_POINT('Ctrl Pts',(-6.59120306404331,-7.00141528186886,-1.));
#5891=CARTESIAN_POINT('Ctrl Pts',(-6.60587239994886,-7.05836882883083,-1.));
#5892=CARTESIAN_POINT('Ctrl Pts',(-6.61987066605911,-7.11571241317029,-1.));
#5893=CARTESIAN_POINT('Ctrl Pts',(-6.63322107969569,-7.17342042004755,-1.));
#5894=CARTESIAN_POINT('Ctrl Pts',(-6.64593535561053,-7.23147652896402,-1.));
#5895=CARTESIAN_POINT('Ctrl Pts',(-6.65801638970246,-7.28987157005223,-1.));
#5896=CARTESIAN_POINT('Ctrl Pts',(-6.66946176275798,-7.34860073021491,-1.));
#5897=CARTESIAN_POINT('Ctrl Pts',(-6.68026694677668,-7.40766099640557,-1.));
#5898=CARTESIAN_POINT('Ctrl Pts',(-6.69042862091104,-7.46704851290034,-1.));
#5899=CARTESIAN_POINT('Ctrl Pts',(-6.69994799095524,-7.52675593674632,-1.));
#5900=CARTESIAN_POINT('Ctrl Pts',(-6.70882947565318,-7.58677347699225,-1.));
#5901=CARTESIAN_POINT('Ctrl Pts',(-6.71707933277187,-7.64708998288989,-1.));
#5902=CARTESIAN_POINT('Ctrl Pts',(-6.72470431659336,-7.70769400824502,-1.));
#5903=CARTESIAN_POINT('Ctrl Pts',(-6.73171032576036,-7.76857488460783,-1.));
#5904=CARTESIAN_POINT('Ctrl Pts',(-6.73810106562749,-7.82972378407324,-1.));
#5905=CARTESIAN_POINT('Ctrl Pts',(-6.74387863902608,-7.89113323756912,-1.));
#5906=CARTESIAN_POINT('Ctrl Pts',(-6.74904413083761,-7.95279665937613,-1.));
#5907=CARTESIAN_POINT('Ctrl Pts',(-6.75359819949755,-8.01470786732018,-1.));
#5908=CARTESIAN_POINT('Ctrl Pts',(-6.7575416648609,-8.07686060726827,-1.));
#5909=CARTESIAN_POINT('Ctrl Pts',(-6.76087611417306,-8.13924806419107,-1.));
#5910=CARTESIAN_POINT('Ctrl Pts',(-6.7636036696164,-8.20186305794854,-1.));
#5911=CARTESIAN_POINT('Ctrl Pts',(-6.76572674650935,-8.26469824786602,-1.));
#5912=CARTESIAN_POINT('Ctrl Pts',(-6.76724781676282,-8.32774633509908,-1.));
#5913=CARTESIAN_POINT('Ctrl Pts',(-6.76816918165128,-8.39100025749018,-1.));
#5914=CARTESIAN_POINT('Ctrl Pts',(-6.76849272647566,-8.45445340444926,-1.));
#5915=CARTESIAN_POINT('Ctrl Pts',(-6.76822000004555,-8.51809951610773,-1.));
#5916=CARTESIAN_POINT('Ctrl Pts',(-6.76735232235635,-8.58193255779939,-1.));
#5917=CARTESIAN_POINT('Ctrl Pts',(-6.76589088878266,-8.64594659806298,-1.));
#5918=CARTESIAN_POINT('Ctrl Pts',(-6.76383687353853,-8.71013569385599,-1.));
#5919=CARTESIAN_POINT('Ctrl Pts',(-6.76119155448275,-8.77449374557664,-1.));
#5920=CARTESIAN_POINT('Ctrl Pts',(-6.7579562951925,-8.8390145737747,-1.));
#5921=CARTESIAN_POINT('Ctrl Pts',(-6.75413249860576,-8.90369203916217,-1.));
#5922=CARTESIAN_POINT('Ctrl Pts',(-6.7497215739923,-8.96852015431046,-1.));
#5923=CARTESIAN_POINT('Ctrl Pts',(-6.74472490424423,-9.03349318036198,-1.));
#5924=CARTESIAN_POINT('Ctrl Pts',(-6.73914381348524,-9.09860577342165,-1.));
#5925=CARTESIAN_POINT('Ctrl Pts',(-6.73297955932548,-9.16385288053588,-1.));
#5926=CARTESIAN_POINT('Ctrl Pts',(-6.72623333926846,-9.22922952332025,-1.));
#5927=CARTESIAN_POINT('Ctrl Pts',(-6.71890629646187,-9.2947306015555,-1.));
#5928=CARTESIAN_POINT('Ctrl Pts',(-6.71099953007124,-9.36035072031876,-1.));
#5929=CARTESIAN_POINT('Ctrl Pts',(-6.7025141076082,-9.42608392519666,-1.));
#5930=CARTESIAN_POINT('Ctrl Pts',(-6.69345108162377,-9.49192378686253,-1.));
#5931=CARTESIAN_POINT('Ctrl Pts',(-6.68381150859183,-9.55786385494286,-1.));
#5932=CARTESIAN_POINT('Ctrl Pts',(-6.67359647366962,-9.62389802250187,-1.));
#5933=CARTESIAN_POINT('Ctrl Pts',(-6.6628071116072,-9.69002090483257,-1.));
#5934=CARTESIAN_POINT('Ctrl Pts',(-6.65144464725859,-9.75622826411013,-1.));
#5935=CARTESIAN_POINT('Ctrl Pts',(-6.63951038900667,-9.82251725114898,-1.));
#5936=CARTESIAN_POINT('Ctrl Pts',(-6.62700557693596,-9.88888607996273,-1.));
#5937=CARTESIAN_POINT('Ctrl Pts',(-6.61654612354184,-9.94204425953052,-1.));
#5938=CARTESIAN_POINT('Ctrl Pts',(-6.60844558393657,-9.98194823089968,-1.));
#5939=CARTESIAN_POINT('Ctrl Pts',(-6.60293150665659,-10.0085665785717,-1.));
#5940=CARTESIAN_POINT('Ctrl Pts',(-6.60014603862878,-10.0218796774244,-1.));
#5941=CARTESIAN_POINT('Ctrl Pts',(-6.06863042059311,-5.89037560471066,6.));
#5942=CARTESIAN_POINT('Ctrl Pts',(-6.076421189359,-5.89793753402584,6.));
#5943=CARTESIAN_POINT('Ctrl Pts',(-6.09164867072824,-5.91336588048663,6.));
#5944=CARTESIAN_POINT('Ctrl Pts',(-6.11342775487885,-5.93742183851679,6.));
#5945=CARTESIAN_POINT('Ctrl Pts',(-6.14045331140034,-5.97123031969246,6.));
#5946=CARTESIAN_POINT('Ctrl Pts',(-6.17151878498999,-6.01584411654483,6.));
#5947=CARTESIAN_POINT('Ctrl Pts',(-6.20066685685755,-6.06213722636286,6.));
#5948=CARTESIAN_POINT('Ctrl Pts',(-6.22866991793492,-6.10945353793713,6.));
#5949=CARTESIAN_POINT('Ctrl Pts',(-6.25605474467853,-6.15733614814835,6.));
#5950=CARTESIAN_POINT('Ctrl Pts',(-6.28297985424308,-6.20562962932064,6.));
#5951=CARTESIAN_POINT('Ctrl Pts',(-6.30937750420801,-6.2543646376197,6.));
#5952=CARTESIAN_POINT('Ctrl Pts',(-6.33505137069502,-6.30367904881886,6.));
#5953=CARTESIAN_POINT('Ctrl Pts',(-6.35978286360965,-6.35373180396276,6.));
#5954=CARTESIAN_POINT('Ctrl Pts',(-6.38345478017076,-6.40460296268299,6.));
#5955=CARTESIAN_POINT('Ctrl Pts',(-6.40608444337878,-6.45626649182452,6.));
#5956=CARTESIAN_POINT('Ctrl Pts',(-6.42776254872514,-6.50863892931076,6.));
#5957=CARTESIAN_POINT('Ctrl Pts',(-6.44861636238489,-6.56160843323027,6.));
#5958=CARTESIAN_POINT('Ctrl Pts',(-6.46876645798849,-6.6150690793574,6.));
#5959=CARTESIAN_POINT('Ctrl Pts',(-6.48827758470623,-6.66895976394943,6.));
#5960=CARTESIAN_POINT('Ctrl Pts',(-6.50715912032692,-6.72326378902151,6.));
#5961=CARTESIAN_POINT('Ctrl Pts',(-6.52538888693356,-6.77798990345396,6.));
#5962=CARTESIAN_POINT('Ctrl Pts',(-6.54292981913304,-6.83315901897031,6.));
#5963=CARTESIAN_POINT('Ctrl Pts',(-6.5597485722992,-6.88878938806037,6.));
#5964=CARTESIAN_POINT('Ctrl Pts',(-6.57583595416561,-6.94488033148853,6.));
#5965=CARTESIAN_POINT('Ctrl Pts',(-6.59120306404331,-7.00141528186886,6.));
#5966=CARTESIAN_POINT('Ctrl Pts',(-6.60587239994886,-7.05836882883083,6.));
#5967=CARTESIAN_POINT('Ctrl Pts',(-6.61987066605911,-7.11571241317029,6.));
#5968=CARTESIAN_POINT('Ctrl Pts',(-6.63322107969569,-7.17342042004755,6.));
#5969=CARTESIAN_POINT('Ctrl Pts',(-6.64593535561053,-7.23147652896402,6.));
#5970=CARTESIAN_POINT('Ctrl Pts',(-6.65801638970246,-7.28987157005223,6.));
#5971=CARTESIAN_POINT('Ctrl Pts',(-6.66946176275798,-7.34860073021491,6.));
#5972=CARTESIAN_POINT('Ctrl Pts',(-6.68026694677668,-7.40766099640557,6.));
#5973=CARTESIAN_POINT('Ctrl Pts',(-6.69042862091104,-7.46704851290034,6.));
#5974=CARTESIAN_POINT('Ctrl Pts',(-6.69994799095524,-7.52675593674632,6.));
#5975=CARTESIAN_POINT('Ctrl Pts',(-6.70882947565318,-7.58677347699225,6.));
#5976=CARTESIAN_POINT('Ctrl Pts',(-6.71707933277187,-7.64708998288989,6.));
#5977=CARTESIAN_POINT('Ctrl Pts',(-6.72470431659336,-7.70769400824502,6.));
#5978=CARTESIAN_POINT('Ctrl Pts',(-6.73171032576036,-7.76857488460783,6.));
#5979=CARTESIAN_POINT('Ctrl Pts',(-6.73810106562749,-7.82972378407324,6.));
#5980=CARTESIAN_POINT('Ctrl Pts',(-6.74387863902608,-7.89113323756912,6.));
#5981=CARTESIAN_POINT('Ctrl Pts',(-6.74904413083761,-7.95279665937613,6.));
#5982=CARTESIAN_POINT('Ctrl Pts',(-6.75359819949755,-8.01470786732018,6.));
#5983=CARTESIAN_POINT('Ctrl Pts',(-6.7575416648609,-8.07686060726827,6.));
#5984=CARTESIAN_POINT('Ctrl Pts',(-6.76087611417306,-8.13924806419107,6.));
#5985=CARTESIAN_POINT('Ctrl Pts',(-6.7636036696164,-8.20186305794854,6.));
#5986=CARTESIAN_POINT('Ctrl Pts',(-6.76572674650935,-8.26469824786602,6.));
#5987=CARTESIAN_POINT('Ctrl Pts',(-6.76724781676282,-8.32774633509908,6.));
#5988=CARTESIAN_POINT('Ctrl Pts',(-6.76816918165128,-8.39100025749018,6.));
#5989=CARTESIAN_POINT('Ctrl Pts',(-6.76849272647566,-8.45445340444926,6.));
#5990=CARTESIAN_POINT('Ctrl Pts',(-6.76822000004555,-8.51809951610773,6.));
#5991=CARTESIAN_POINT('Ctrl Pts',(-6.76735232235635,-8.58193255779939,6.));
#5992=CARTESIAN_POINT('Ctrl Pts',(-6.76589088878266,-8.64594659806298,6.));
#5993=CARTESIAN_POINT('Ctrl Pts',(-6.76383687353853,-8.71013569385599,6.));
#5994=CARTESIAN_POINT('Ctrl Pts',(-6.76119155448275,-8.77449374557664,6.));
#5995=CARTESIAN_POINT('Ctrl Pts',(-6.7579562951925,-8.8390145737747,6.));
#5996=CARTESIAN_POINT('Ctrl Pts',(-6.75413249860576,-8.90369203916217,6.));
#5997=CARTESIAN_POINT('Ctrl Pts',(-6.7497215739923,-8.96852015431046,6.));
#5998=CARTESIAN_POINT('Ctrl Pts',(-6.74472490424423,-9.03349318036198,6.));
#5999=CARTESIAN_POINT('Ctrl Pts',(-6.73914381348524,-9.09860577342165,6.));
#6000=CARTESIAN_POINT('Ctrl Pts',(-6.73297955932548,-9.16385288053588,6.));
#6001=CARTESIAN_POINT('Ctrl Pts',(-6.72623333926846,-9.22922952332025,6.));
#6002=CARTESIAN_POINT('Ctrl Pts',(-6.71890629646187,-9.2947306015555,6.));
#6003=CARTESIAN_POINT('Ctrl Pts',(-6.71099953007124,-9.36035072031876,6.));
#6004=CARTESIAN_POINT('Ctrl Pts',(-6.7025141076082,-9.42608392519666,6.));
#6005=CARTESIAN_POINT('Ctrl Pts',(-6.69345108162377,-9.49192378686253,6.));
#6006=CARTESIAN_POINT('Ctrl Pts',(-6.68381150859183,-9.55786385494286,6.));
#6007=CARTESIAN_POINT('Ctrl Pts',(-6.67359647366962,-9.62389802250187,6.));
#6008=CARTESIAN_POINT('Ctrl Pts',(-6.6628071116072,-9.69002090483257,6.));
#6009=CARTESIAN_POINT('Ctrl Pts',(-6.65144464725859,-9.75622826411013,6.));
#6010=CARTESIAN_POINT('Ctrl Pts',(-6.63951038900667,-9.82251725114898,6.));
#6011=CARTESIAN_POINT('Ctrl Pts',(-6.62700557693596,-9.88888607996273,6.));
#6012=CARTESIAN_POINT('Ctrl Pts',(-6.61654612354184,-9.94204425953052,6.));
#6013=CARTESIAN_POINT('Ctrl Pts',(-6.60844558393657,-9.98194823089968,6.));
#6014=CARTESIAN_POINT('Ctrl Pts',(-6.60293150665659,-10.0085665785717,6.));
#6015=CARTESIAN_POINT('Ctrl Pts',(-6.60014603862878,-10.0218796774244,6.));
#6016=CARTESIAN_POINT('Ctrl Pts',(-11.9792754136349,-0.704954299427526,
-3.75));
#6017=CARTESIAN_POINT('Ctrl Pts',(-11.9792754136349,-0.704954299427526,
12.75));
#6018=CARTESIAN_POINT('Ctrl Pts',(-11.9691386658393,-0.71402313492741,-3.75));
#6019=CARTESIAN_POINT('Ctrl Pts',(-11.9691386658393,-0.71402313492741,12.75));
#6020=CARTESIAN_POINT('Ctrl Pts',(-11.9488435391885,-0.732107639766307,
-3.75));
#6021=CARTESIAN_POINT('Ctrl Pts',(-11.9488435391885,-0.732107639766307,
12.75));
#6022=CARTESIAN_POINT('Ctrl Pts',(-11.9183359560736,-0.759074898533417,
-3.75));
#6023=CARTESIAN_POINT('Ctrl Pts',(-11.9183359560736,-0.759074898533417,
12.75));
#6024=CARTESIAN_POINT('Ctrl Pts',(-11.877529348846,-0.794712140666323,-3.75));
#6025=CARTESIAN_POINT('Ctrl Pts',(-11.877529348846,-0.794712140666323,12.75));
#6026=CARTESIAN_POINT('Ctrl Pts',(-11.8263046631092,-0.838726039995981,
-3.75));
#6027=CARTESIAN_POINT('Ctrl Pts',(-11.8263046631092,-0.838726039995981,
12.75));
#6028=CARTESIAN_POINT('Ctrl Pts',(-11.7748638454684,-0.882205904336895,
-3.75));
#6029=CARTESIAN_POINT('Ctrl Pts',(-11.7748638454684,-0.882205904336895,
12.75));
#6030=CARTESIAN_POINT('Ctrl Pts',(-11.7232078225909,-0.925149766751159,
-3.75));
#6031=CARTESIAN_POINT('Ctrl Pts',(-11.7232078225909,-0.925149766751159,
12.75));
#6032=CARTESIAN_POINT('Ctrl Pts',(-11.6713384077523,-0.96755506955319,-3.75));
#6033=CARTESIAN_POINT('Ctrl Pts',(-11.6713384077523,-0.96755506955319,12.75));
#6034=CARTESIAN_POINT('Ctrl Pts',(-11.6192586585895,-1.00941863307588,-3.75));
#6035=CARTESIAN_POINT('Ctrl Pts',(-11.6192586585895,-1.00941863307588,12.75));
#6036=CARTESIAN_POINT('Ctrl Pts',(-11.5669726710206,-1.05073678224334,-3.75));
#6037=CARTESIAN_POINT('Ctrl Pts',(-11.5669726710206,-1.05073678224334,12.75));
#6038=CARTESIAN_POINT('Ctrl Pts',(-11.5144851912285,-1.09150552381395,-3.75));
#6039=CARTESIAN_POINT('Ctrl Pts',(-11.5144851912285,-1.09150552381395,12.75));
#6040=CARTESIAN_POINT('Ctrl Pts',(-11.4618012771636,-1.13172071766774,-3.75));
#6041=CARTESIAN_POINT('Ctrl Pts',(-11.4618012771636,-1.13172071766774,12.75));
#6042=CARTESIAN_POINT('Ctrl Pts',(-11.4089259705106,-1.17137823760544,-3.75));
#6043=CARTESIAN_POINT('Ctrl Pts',(-11.4089259705106,-1.17137823760544,12.75));
#6044=CARTESIAN_POINT('Ctrl Pts',(-11.3558638941869,-1.21047418192819,-3.75));
#6045=CARTESIAN_POINT('Ctrl Pts',(-11.3558638941869,-1.21047418192819,12.75));
#6046=CARTESIAN_POINT('Ctrl Pts',(-11.30261917075,-1.24900490126927,-3.75));
#6047=CARTESIAN_POINT('Ctrl Pts',(-11.30261917075,-1.24900490126927,12.75));
#6048=CARTESIAN_POINT('Ctrl Pts',(-11.2491956455455,-1.28696685552412,-3.75));
#6049=CARTESIAN_POINT('Ctrl Pts',(-11.2491956455455,-1.28696685552412,12.75));
#6050=CARTESIAN_POINT('Ctrl Pts',(-11.1955970312291,-1.32435651843207,-3.75));
#6051=CARTESIAN_POINT('Ctrl Pts',(-11.1955970312291,-1.32435651843207,12.75));
#6052=CARTESIAN_POINT('Ctrl Pts',(-11.1418270749817,-1.36117027439398,-3.75));
#6053=CARTESIAN_POINT('Ctrl Pts',(-11.1418270749817,-1.36117027439398,12.75));
#6054=CARTESIAN_POINT('Ctrl Pts',(-11.0878897426906,-1.39740430473756,-3.75));
#6055=CARTESIAN_POINT('Ctrl Pts',(-11.0878897426906,-1.39740430473756,12.75));
#6056=CARTESIAN_POINT('Ctrl Pts',(-11.033789312906,-1.43305454241432,-3.75));
#6057=CARTESIAN_POINT('Ctrl Pts',(-11.033789312906,-1.43305454241432,12.75));
#6058=CARTESIAN_POINT('Ctrl Pts',(-10.9795302662584,-1.46811677324654,-3.75));
#6059=CARTESIAN_POINT('Ctrl Pts',(-10.9795302662584,-1.46811677324654,12.75));
#6060=CARTESIAN_POINT('Ctrl Pts',(-10.9251172180581,-1.50258671261028,-3.75));
#6061=CARTESIAN_POINT('Ctrl Pts',(-10.9251172180581,-1.50258671261028,12.75));
#6062=CARTESIAN_POINT('Ctrl Pts',(-10.8705548380775,-1.53646008988796,-3.75));
#6063=CARTESIAN_POINT('Ctrl Pts',(-10.8705548380775,-1.53646008988796,12.75));
#6064=CARTESIAN_POINT('Ctrl Pts',(-10.8158477697972,-1.56973274862051,-3.75));
#6065=CARTESIAN_POINT('Ctrl Pts',(-10.8158477697972,-1.56973274862051,12.75));
#6066=CARTESIAN_POINT('Ctrl Pts',(-10.761000572936,-1.60240070038749,-3.75));
#6067=CARTESIAN_POINT('Ctrl Pts',(-10.761000572936,-1.60240070038749,12.75));
#6068=CARTESIAN_POINT('Ctrl Pts',(-10.7060177866027,-1.63445994423348,-3.75));
#6069=CARTESIAN_POINT('Ctrl Pts',(-10.7060177866027,-1.63445994423348,12.75));
#6070=CARTESIAN_POINT('Ctrl Pts',(-10.6509039769739,-1.66590631967585,-3.75));
#6071=CARTESIAN_POINT('Ctrl Pts',(-10.6509039769739,-1.66590631967585,12.75));
#6072=CARTESIAN_POINT('Ctrl Pts',(-10.59566379085,-1.69673535547184,-3.75));
#6073=CARTESIAN_POINT('Ctrl Pts',(-10.59566379085,-1.69673535547184,12.75));
#6074=CARTESIAN_POINT('Ctrl Pts',(-10.5403020105194,-1.72694211360792,-3.75));
#6075=CARTESIAN_POINT('Ctrl Pts',(-10.5403020105194,-1.72694211360792,12.75));
#6076=CARTESIAN_POINT('Ctrl Pts',(-10.4848236013528,-1.75652107004318,-3.75));
#6077=CARTESIAN_POINT('Ctrl Pts',(-10.4848236013528,-1.75652107004318,12.75));
#6078=CARTESIAN_POINT('Ctrl Pts',(-10.4292336483793,-1.78546643461775,-3.75));
#6079=CARTESIAN_POINT('Ctrl Pts',(-10.4292336483793,-1.78546643461775,12.75));
#6080=CARTESIAN_POINT('Ctrl Pts',(-10.3735373011506,-1.81377244526718,-3.75));
#6081=CARTESIAN_POINT('Ctrl Pts',(-10.3735373011506,-1.81377244526718,12.75));
#6082=CARTESIAN_POINT('Ctrl Pts',(-10.317739716759,-1.84143367405762,-3.75));
#6083=CARTESIAN_POINT('Ctrl Pts',(-10.317739716759,-1.84143367405762,12.75));
#6084=CARTESIAN_POINT('Ctrl Pts',(-10.2618460035706,-1.86844533887956,-3.75));
#6085=CARTESIAN_POINT('Ctrl Pts',(-10.2618460035706,-1.86844533887956,12.75));
#6086=CARTESIAN_POINT('Ctrl Pts',(-10.2058611678956,-1.89480360265125,-3.75));
#6087=CARTESIAN_POINT('Ctrl Pts',(-10.2058611678956,-1.89480360265125,12.75));
#6088=CARTESIAN_POINT('Ctrl Pts',(-10.1497902344364,-1.92050480406378,-3.75));
#6089=CARTESIAN_POINT('Ctrl Pts',(-10.1497902344364,-1.92050480406378,12.75));
#6090=CARTESIAN_POINT('Ctrl Pts',(-10.0936383641523,-1.94554471072257,-3.75));
#6091=CARTESIAN_POINT('Ctrl Pts',(-10.0936383641523,-1.94554471072257,12.75));
#6092=CARTESIAN_POINT('Ctrl Pts',(-10.037410974034,-1.96991776698621,-3.75));
#6093=CARTESIAN_POINT('Ctrl Pts',(-10.037410974034,-1.96991776698621,12.75));
#6094=CARTESIAN_POINT('Ctrl Pts',(-9.98111385659409,-1.99361634997092,-3.75));
#6095=CARTESIAN_POINT('Ctrl Pts',(-9.98111385659409,-1.99361634997092,12.75));
#6096=CARTESIAN_POINT('Ctrl Pts',(-9.92475330165988,-2.01663001707736,-3.75));
#6097=CARTESIAN_POINT('Ctrl Pts',(-9.92475330165988,-2.01663001707736,12.75));
#6098=CARTESIAN_POINT('Ctrl Pts',(-9.86833584478527,-2.03894719582858,-3.75));
#6099=CARTESIAN_POINT('Ctrl Pts',(-9.86833584478527,-2.03894719582858,12.75));
#6100=CARTESIAN_POINT('Ctrl Pts',(-9.81186801391803,-2.06055689146527,-3.75));
#6101=CARTESIAN_POINT('Ctrl Pts',(-9.81186801391803,-2.06055689146527,12.75));
#6102=CARTESIAN_POINT('Ctrl Pts',(-9.75535607889872,-2.08145038176732,-3.75));
#6103=CARTESIAN_POINT('Ctrl Pts',(-9.75535607889872,-2.08145038176732,12.75));
#6104=CARTESIAN_POINT('Ctrl Pts',(-9.69880579601398,-2.10162295100989,-3.75));
#6105=CARTESIAN_POINT('Ctrl Pts',(-9.69880579601398,-2.10162295100989,12.75));
#6106=CARTESIAN_POINT('Ctrl Pts',(-9.64222216484242,-2.12107554726937,-3.75));
#6107=CARTESIAN_POINT('Ctrl Pts',(-9.64222216484242,-2.12107554726937,12.75));
#6108=CARTESIAN_POINT('Ctrl Pts',(-9.58561005875903,-2.13981058538587,-3.75));
#6109=CARTESIAN_POINT('Ctrl Pts',(-9.58561005875903,-2.13981058538587,12.75));
#6110=CARTESIAN_POINT('Ctrl Pts',(-9.52897485563507,-2.15782775391113,-3.75));
#6111=CARTESIAN_POINT('Ctrl Pts',(-9.52897485563507,-2.15782775391113,12.75));
#6112=CARTESIAN_POINT('Ctrl Pts',(-9.4723230488593,-2.17511995998945,-3.75));
#6113=CARTESIAN_POINT('Ctrl Pts',(-9.4723230488593,-2.17511995998945,12.75));
#6114=CARTESIAN_POINT('Ctrl Pts',(-9.41566291502215,-2.19166889809876,-3.75));
#6115=CARTESIAN_POINT('Ctrl Pts',(-9.41566291502215,-2.19166889809876,12.75));
#6116=CARTESIAN_POINT('Ctrl Pts',(-9.35900502856467,-2.2074416540289,-3.75));
#6117=CARTESIAN_POINT('Ctrl Pts',(-9.35900502856467,-2.2074416540289,12.75));
#6118=CARTESIAN_POINT('Ctrl Pts',(-9.30236077039477,-2.22240082168223,-3.75));
#6119=CARTESIAN_POINT('Ctrl Pts',(-9.30236077039477,-2.22240082168223,12.75));
#6120=CARTESIAN_POINT('Ctrl Pts',(-9.24574089753054,-2.23651421201962,-3.75));
#6121=CARTESIAN_POINT('Ctrl Pts',(-9.24574089753054,-2.23651421201962,12.75));
#6122=CARTESIAN_POINT('Ctrl Pts',(-9.18915420809356,-2.24976392906278,-3.75));
#6123=CARTESIAN_POINT('Ctrl Pts',(-9.18915420809356,-2.24976392906278,12.75));
#6124=CARTESIAN_POINT('Ctrl Pts',(-9.13260588645235,-2.26215759393014,-3.75));
#6125=CARTESIAN_POINT('Ctrl Pts',(-9.13260588645235,-2.26215759393014,12.75));
#6126=CARTESIAN_POINT('Ctrl Pts',(-9.07609679780011,-2.27373321015996,-3.75));
#6127=CARTESIAN_POINT('Ctrl Pts',(-9.07609679780011,-2.27373321015996,12.75));
#6128=CARTESIAN_POINT('Ctrl Pts',(-9.0196273647496,-2.28453333318601,-3.75));
#6129=CARTESIAN_POINT('Ctrl Pts',(-9.0196273647496,-2.28453333318601,12.75));
#6130=CARTESIAN_POINT('Ctrl Pts',(-8.96320109950669,-2.29458154408801,-3.75));
#6131=CARTESIAN_POINT('Ctrl Pts',(-8.96320109950669,-2.29458154408801,12.75));
#6132=CARTESIAN_POINT('Ctrl Pts',(-8.90682777405608,-2.30386137247017,-3.75));
#6133=CARTESIAN_POINT('Ctrl Pts',(-8.90682777405608,-2.30386137247017,12.75));
#6134=CARTESIAN_POINT('Ctrl Pts',(-8.85052793120604,-2.31228619203479,-3.75));
#6135=CARTESIAN_POINT('Ctrl Pts',(-8.85052793120604,-2.31228619203479,12.75));
#6136=CARTESIAN_POINT('Ctrl Pts',(-8.79433301721166,-2.31969862084206,-3.75));
#6137=CARTESIAN_POINT('Ctrl Pts',(-8.79433301721166,-2.31969862084206,12.75));
#6138=CARTESIAN_POINT('Ctrl Pts',(-8.73827625692193,-2.32593252219559,-3.75));
#6139=CARTESIAN_POINT('Ctrl Pts',(-8.73827625692193,-2.32593252219559,12.75));
#6140=CARTESIAN_POINT('Ctrl Pts',(-8.68238458286971,-2.33086762045752,-3.75));
#6141=CARTESIAN_POINT('Ctrl Pts',(-8.68238458286971,-2.33086762045752,12.75));
#6142=CARTESIAN_POINT('Ctrl Pts',(-8.62667187892838,-2.33447589689188,-3.75));
#6143=CARTESIAN_POINT('Ctrl Pts',(-8.62667187892838,-2.33447589689188,12.75));
#6144=CARTESIAN_POINT('Ctrl Pts',(-8.57112741281372,-2.33689888190034,-3.75));
#6145=CARTESIAN_POINT('Ctrl Pts',(-8.57112741281372,-2.33689888190034,12.75));
#6146=CARTESIAN_POINT('Ctrl Pts',(-8.51572283259063,-2.33840535058003,-3.75));
#6147=CARTESIAN_POINT('Ctrl Pts',(-8.51572283259063,-2.33840535058003,12.75));
#6148=CARTESIAN_POINT('Ctrl Pts',(-8.46043689627597,-2.3392342622836,-3.75));
#6149=CARTESIAN_POINT('Ctrl Pts',(-8.46043689627597,-2.3392342622836,12.75));
#6150=CARTESIAN_POINT('Ctrl Pts',(-8.40527692606173,-2.339459611751,-3.75));
#6151=CARTESIAN_POINT('Ctrl Pts',(-8.40527692606173,-2.339459611751,12.75));
#6152=CARTESIAN_POINT('Ctrl Pts',(-8.35029826768635,-2.33886640526141,-3.75));
#6153=CARTESIAN_POINT('Ctrl Pts',(-8.35029826768635,-2.33886640526141,12.75));
#6154=CARTESIAN_POINT('Ctrl Pts',(-8.29563322262998,-2.33676998946178,-3.75));
#6155=CARTESIAN_POINT('Ctrl Pts',(-8.29563322262998,-2.33676998946178,12.75));
#6156=CARTESIAN_POINT('Ctrl Pts',(-8.24146380440172,-2.33217339857873,-3.75));
#6157=CARTESIAN_POINT('Ctrl Pts',(-8.24146380440172,-2.33217339857873,12.75));
#6158=CARTESIAN_POINT('Ctrl Pts',(-8.19867202257948,-2.32567282066755,-3.75));
#6159=CARTESIAN_POINT('Ctrl Pts',(-8.19867202257948,-2.32567282066755,12.75));
#6160=CARTESIAN_POINT('Ctrl Pts',(-8.16694940973768,-2.31883955953704,-3.75));
#6161=CARTESIAN_POINT('Ctrl Pts',(-8.16694940973768,-2.31883955953704,12.75));
#6162=CARTESIAN_POINT('Ctrl Pts',(-8.14597432907962,-2.31336634706602,-3.75));
#6163=CARTESIAN_POINT('Ctrl Pts',(-8.14597432907962,-2.31336634706602,12.75));
#6164=CARTESIAN_POINT('Ctrl Pts',(-8.13553012180811,-2.31040030805734,-3.75));
#6165=CARTESIAN_POINT('Ctrl Pts',(-8.13553012180811,-2.31040030805734,12.75));
#6166=CARTESIAN_POINT('',(-11.9792754136349,-0.704954299427494,-1.));
#6167=CARTESIAN_POINT('Ctrl Pts',(-11.9792754136349,-0.704954299427526,
-1.));
#6168=CARTESIAN_POINT('Ctrl Pts',(-11.9691386658393,-0.71402313492741,-1.));
#6169=CARTESIAN_POINT('Ctrl Pts',(-11.9488435391885,-0.732107639766307,
-1.));
#6170=CARTESIAN_POINT('Ctrl Pts',(-11.9183359560736,-0.759074898533417,
-1.));
#6171=CARTESIAN_POINT('Ctrl Pts',(-11.877529348846,-0.794712140666323,-1.));
#6172=CARTESIAN_POINT('Ctrl Pts',(-11.8263046631092,-0.838726039995981,
-1.));
#6173=CARTESIAN_POINT('Ctrl Pts',(-11.7748638454684,-0.882205904336895,
-1.));
#6174=CARTESIAN_POINT('Ctrl Pts',(-11.7232078225909,-0.925149766751159,
-1.));
#6175=CARTESIAN_POINT('Ctrl Pts',(-11.6713384077523,-0.96755506955319,-1.));
#6176=CARTESIAN_POINT('Ctrl Pts',(-11.6192586585895,-1.00941863307588,-1.));
#6177=CARTESIAN_POINT('Ctrl Pts',(-11.5669726710206,-1.05073678224334,-1.));
#6178=CARTESIAN_POINT('Ctrl Pts',(-11.5144851912285,-1.09150552381395,-1.));
#6179=CARTESIAN_POINT('Ctrl Pts',(-11.4618012771636,-1.13172071766774,-1.));
#6180=CARTESIAN_POINT('Ctrl Pts',(-11.4089259705106,-1.17137823760544,-1.));
#6181=CARTESIAN_POINT('Ctrl Pts',(-11.3558638941869,-1.21047418192819,-1.));
#6182=CARTESIAN_POINT('Ctrl Pts',(-11.30261917075,-1.24900490126927,-1.));
#6183=CARTESIAN_POINT('Ctrl Pts',(-11.2491956455455,-1.28696685552412,-1.));
#6184=CARTESIAN_POINT('Ctrl Pts',(-11.1955970312291,-1.32435651843207,-1.));
#6185=CARTESIAN_POINT('Ctrl Pts',(-11.1418270749817,-1.36117027439398,-1.));
#6186=CARTESIAN_POINT('Ctrl Pts',(-11.0878897426906,-1.39740430473756,-1.));
#6187=CARTESIAN_POINT('Ctrl Pts',(-11.033789312906,-1.43305454241432,-1.));
#6188=CARTESIAN_POINT('Ctrl Pts',(-10.9795302662584,-1.46811677324654,-1.));
#6189=CARTESIAN_POINT('Ctrl Pts',(-10.9251172180581,-1.50258671261028,-1.));
#6190=CARTESIAN_POINT('Ctrl Pts',(-10.8705548380775,-1.53646008988796,-1.));
#6191=CARTESIAN_POINT('Ctrl Pts',(-10.8158477697972,-1.56973274862051,-1.));
#6192=CARTESIAN_POINT('Ctrl Pts',(-10.761000572936,-1.60240070038749,-1.));
#6193=CARTESIAN_POINT('Ctrl Pts',(-10.7060177866027,-1.63445994423348,-1.));
#6194=CARTESIAN_POINT('Ctrl Pts',(-10.6509039769739,-1.66590631967585,-1.));
#6195=CARTESIAN_POINT('Ctrl Pts',(-10.59566379085,-1.69673535547184,-1.));
#6196=CARTESIAN_POINT('Ctrl Pts',(-10.5403020105194,-1.72694211360792,-1.));
#6197=CARTESIAN_POINT('Ctrl Pts',(-10.4848236013528,-1.75652107004318,-1.));
#6198=CARTESIAN_POINT('Ctrl Pts',(-10.4292336483793,-1.78546643461775,-1.));
#6199=CARTESIAN_POINT('Ctrl Pts',(-10.3735373011506,-1.81377244526718,-1.));
#6200=CARTESIAN_POINT('Ctrl Pts',(-10.317739716759,-1.84143367405762,-1.));
#6201=CARTESIAN_POINT('Ctrl Pts',(-10.2618460035706,-1.86844533887956,-1.));
#6202=CARTESIAN_POINT('Ctrl Pts',(-10.2058611678956,-1.89480360265125,-1.));
#6203=CARTESIAN_POINT('Ctrl Pts',(-10.1497902344364,-1.92050480406378,-1.));
#6204=CARTESIAN_POINT('Ctrl Pts',(-10.0936383641523,-1.94554471072257,-1.));
#6205=CARTESIAN_POINT('Ctrl Pts',(-10.037410974034,-1.96991776698621,-1.));
#6206=CARTESIAN_POINT('Ctrl Pts',(-9.98111385659409,-1.99361634997092,-1.));
#6207=CARTESIAN_POINT('Ctrl Pts',(-9.92475330165988,-2.01663001707736,-1.));
#6208=CARTESIAN_POINT('Ctrl Pts',(-9.86833584478527,-2.03894719582858,-1.));
#6209=CARTESIAN_POINT('Ctrl Pts',(-9.81186801391803,-2.06055689146527,-1.));
#6210=CARTESIAN_POINT('Ctrl Pts',(-9.75535607889872,-2.08145038176732,-1.));
#6211=CARTESIAN_POINT('Ctrl Pts',(-9.69880579601398,-2.10162295100989,-1.));
#6212=CARTESIAN_POINT('Ctrl Pts',(-9.64222216484242,-2.12107554726937,-1.));
#6213=CARTESIAN_POINT('Ctrl Pts',(-9.58561005875903,-2.13981058538587,-1.));
#6214=CARTESIAN_POINT('Ctrl Pts',(-9.52897485563507,-2.15782775391113,-1.));
#6215=CARTESIAN_POINT('Ctrl Pts',(-9.4723230488593,-2.17511995998945,-1.));
#6216=CARTESIAN_POINT('Ctrl Pts',(-9.41566291502215,-2.19166889809876,-1.));
#6217=CARTESIAN_POINT('Ctrl Pts',(-9.35900502856467,-2.2074416540289,-1.));
#6218=CARTESIAN_POINT('Ctrl Pts',(-9.30236077039477,-2.22240082168223,-1.));
#6219=CARTESIAN_POINT('Ctrl Pts',(-9.24574089753054,-2.23651421201962,-1.));
#6220=CARTESIAN_POINT('Ctrl Pts',(-9.18915420809356,-2.24976392906278,-1.));
#6221=CARTESIAN_POINT('Ctrl Pts',(-9.13260588645235,-2.26215759393014,-1.));
#6222=CARTESIAN_POINT('Ctrl Pts',(-9.07609679780011,-2.27373321015996,-1.));
#6223=CARTESIAN_POINT('Ctrl Pts',(-9.0196273647496,-2.28453333318601,-1.));
#6224=CARTESIAN_POINT('Ctrl Pts',(-8.96320109950669,-2.29458154408801,-1.));
#6225=CARTESIAN_POINT('Ctrl Pts',(-8.90682777405608,-2.30386137247017,-1.));
#6226=CARTESIAN_POINT('Ctrl Pts',(-8.85052793120604,-2.31228619203479,-1.));
#6227=CARTESIAN_POINT('Ctrl Pts',(-8.79433301721166,-2.31969862084206,-1.));
#6228=CARTESIAN_POINT('Ctrl Pts',(-8.73827625692193,-2.32593252219559,-1.));
#6229=CARTESIAN_POINT('Ctrl Pts',(-8.68238458286971,-2.33086762045752,-1.));
#6230=CARTESIAN_POINT('Ctrl Pts',(-8.62667187892838,-2.33447589689188,-1.));
#6231=CARTESIAN_POINT('Ctrl Pts',(-8.57112741281372,-2.33689888190034,-1.));
#6232=CARTESIAN_POINT('Ctrl Pts',(-8.51572283259063,-2.33840535058003,-1.));
#6233=CARTESIAN_POINT('Ctrl Pts',(-8.46043689627597,-2.3392342622836,-1.));
#6234=CARTESIAN_POINT('Ctrl Pts',(-8.40527692606173,-2.339459611751,-1.));
#6235=CARTESIAN_POINT('Ctrl Pts',(-8.35029826768635,-2.33886640526141,-1.));
#6236=CARTESIAN_POINT('Ctrl Pts',(-8.29563322262998,-2.33676998946178,-1.));
#6237=CARTESIAN_POINT('Ctrl Pts',(-8.24146380440172,-2.33217339857873,-1.));
#6238=CARTESIAN_POINT('Ctrl Pts',(-8.19867202257948,-2.32567282066755,-1.));
#6239=CARTESIAN_POINT('Ctrl Pts',(-8.16694940973768,-2.31883955953704,-1.));
#6240=CARTESIAN_POINT('Ctrl Pts',(-8.14597432907962,-2.31336634706602,-1.));
#6241=CARTESIAN_POINT('Ctrl Pts',(-8.13553012180811,-2.31040030805734,-1.));
#6242=CARTESIAN_POINT('',(-11.9792754136349,-0.704954299427494,6.));
#6243=CARTESIAN_POINT('Ctrl Pts',(-11.9792754136349,-0.704954299427526,
6.));
#6244=CARTESIAN_POINT('Ctrl Pts',(-11.9691386658393,-0.71402313492741,6.));
#6245=CARTESIAN_POINT('Ctrl Pts',(-11.9488435391885,-0.732107639766307,
6.));
#6246=CARTESIAN_POINT('Ctrl Pts',(-11.9183359560736,-0.759074898533417,
6.));
#6247=CARTESIAN_POINT('Ctrl Pts',(-11.877529348846,-0.794712140666323,6.));
#6248=CARTESIAN_POINT('Ctrl Pts',(-11.8263046631092,-0.838726039995981,
6.));
#6249=CARTESIAN_POINT('Ctrl Pts',(-11.7748638454684,-0.882205904336895,
6.));
#6250=CARTESIAN_POINT('Ctrl Pts',(-11.7232078225909,-0.925149766751159,
6.));
#6251=CARTESIAN_POINT('Ctrl Pts',(-11.6713384077523,-0.96755506955319,6.));
#6252=CARTESIAN_POINT('Ctrl Pts',(-11.6192586585895,-1.00941863307588,6.));
#6253=CARTESIAN_POINT('Ctrl Pts',(-11.5669726710206,-1.05073678224334,6.));
#6254=CARTESIAN_POINT('Ctrl Pts',(-11.5144851912285,-1.09150552381395,6.));
#6255=CARTESIAN_POINT('Ctrl Pts',(-11.4618012771636,-1.13172071766774,6.));
#6256=CARTESIAN_POINT('Ctrl Pts',(-11.4089259705106,-1.17137823760544,6.));
#6257=CARTESIAN_POINT('Ctrl Pts',(-11.3558638941869,-1.21047418192819,6.));
#6258=CARTESIAN_POINT('Ctrl Pts',(-11.30261917075,-1.24900490126927,6.));
#6259=CARTESIAN_POINT('Ctrl Pts',(-11.2491956455455,-1.28696685552412,6.));
#6260=CARTESIAN_POINT('Ctrl Pts',(-11.1955970312291,-1.32435651843207,6.));
#6261=CARTESIAN_POINT('Ctrl Pts',(-11.1418270749817,-1.36117027439398,6.));
#6262=CARTESIAN_POINT('Ctrl Pts',(-11.0878897426906,-1.39740430473756,6.));
#6263=CARTESIAN_POINT('Ctrl Pts',(-11.033789312906,-1.43305454241432,6.));
#6264=CARTESIAN_POINT('Ctrl Pts',(-10.9795302662584,-1.46811677324654,6.));
#6265=CARTESIAN_POINT('Ctrl Pts',(-10.9251172180581,-1.50258671261028,6.));
#6266=CARTESIAN_POINT('Ctrl Pts',(-10.8705548380775,-1.53646008988796,6.));
#6267=CARTESIAN_POINT('Ctrl Pts',(-10.8158477697972,-1.56973274862051,6.));
#6268=CARTESIAN_POINT('Ctrl Pts',(-10.761000572936,-1.60240070038749,6.));
#6269=CARTESIAN_POINT('Ctrl Pts',(-10.7060177866027,-1.63445994423348,6.));
#6270=CARTESIAN_POINT('Ctrl Pts',(-10.6509039769739,-1.66590631967585,6.));
#6271=CARTESIAN_POINT('Ctrl Pts',(-10.59566379085,-1.69673535547184,6.));
#6272=CARTESIAN_POINT('Ctrl Pts',(-10.5403020105194,-1.72694211360792,6.));
#6273=CARTESIAN_POINT('Ctrl Pts',(-10.4848236013528,-1.75652107004318,6.));
#6274=CARTESIAN_POINT('Ctrl Pts',(-10.4292336483793,-1.78546643461775,6.));
#6275=CARTESIAN_POINT('Ctrl Pts',(-10.3735373011506,-1.81377244526718,6.));
#6276=CARTESIAN_POINT('Ctrl Pts',(-10.317739716759,-1.84143367405762,6.));
#6277=CARTESIAN_POINT('Ctrl Pts',(-10.2618460035706,-1.86844533887956,6.));
#6278=CARTESIAN_POINT('Ctrl Pts',(-10.2058611678956,-1.89480360265125,6.));
#6279=CARTESIAN_POINT('Ctrl Pts',(-10.1497902344364,-1.92050480406378,6.));
#6280=CARTESIAN_POINT('Ctrl Pts',(-10.0936383641523,-1.94554471072257,6.));
#6281=CARTESIAN_POINT('Ctrl Pts',(-10.037410974034,-1.96991776698621,6.));
#6282=CARTESIAN_POINT('Ctrl Pts',(-9.98111385659409,-1.99361634997092,6.));
#6283=CARTESIAN_POINT('Ctrl Pts',(-9.92475330165988,-2.01663001707736,6.));
#6284=CARTESIAN_POINT('Ctrl Pts',(-9.86833584478527,-2.03894719582858,6.));
#6285=CARTESIAN_POINT('Ctrl Pts',(-9.81186801391803,-2.06055689146527,6.));
#6286=CARTESIAN_POINT('Ctrl Pts',(-9.75535607889872,-2.08145038176732,6.));
#6287=CARTESIAN_POINT('Ctrl Pts',(-9.69880579601398,-2.10162295100989,6.));
#6288=CARTESIAN_POINT('Ctrl Pts',(-9.64222216484242,-2.12107554726937,6.));
#6289=CARTESIAN_POINT('Ctrl Pts',(-9.58561005875903,-2.13981058538587,6.));
#6290=CARTESIAN_POINT('Ctrl Pts',(-9.52897485563507,-2.15782775391113,6.));
#6291=CARTESIAN_POINT('Ctrl Pts',(-9.4723230488593,-2.17511995998945,6.));
#6292=CARTESIAN_POINT('Ctrl Pts',(-9.41566291502215,-2.19166889809876,6.));
#6293=CARTESIAN_POINT('Ctrl Pts',(-9.35900502856467,-2.2074416540289,6.));
#6294=CARTESIAN_POINT('Ctrl Pts',(-9.30236077039477,-2.22240082168223,6.));
#6295=CARTESIAN_POINT('Ctrl Pts',(-9.24574089753054,-2.23651421201962,6.));
#6296=CARTESIAN_POINT('Ctrl Pts',(-9.18915420809356,-2.24976392906278,6.));
#6297=CARTESIAN_POINT('Ctrl Pts',(-9.13260588645235,-2.26215759393014,6.));
#6298=CARTESIAN_POINT('Ctrl Pts',(-9.07609679780011,-2.27373321015996,6.));
#6299=CARTESIAN_POINT('Ctrl Pts',(-9.0196273647496,-2.28453333318601,6.));
#6300=CARTESIAN_POINT('Ctrl Pts',(-8.96320109950669,-2.29458154408801,6.));
#6301=CARTESIAN_POINT('Ctrl Pts',(-8.90682777405608,-2.30386137247017,6.));
#6302=CARTESIAN_POINT('Ctrl Pts',(-8.85052793120604,-2.31228619203479,6.));
#6303=CARTESIAN_POINT('Ctrl Pts',(-8.79433301721166,-2.31969862084206,6.));
#6304=CARTESIAN_POINT('Ctrl Pts',(-8.73827625692193,-2.32593252219559,6.));
#6305=CARTESIAN_POINT('Ctrl Pts',(-8.68238458286971,-2.33086762045752,6.));
#6306=CARTESIAN_POINT('Ctrl Pts',(-8.62667187892838,-2.33447589689188,6.));
#6307=CARTESIAN_POINT('Ctrl Pts',(-8.57112741281372,-2.33689888190034,6.));
#6308=CARTESIAN_POINT('Ctrl Pts',(-8.51572283259063,-2.33840535058003,6.));
#6309=CARTESIAN_POINT('Ctrl Pts',(-8.46043689627597,-2.3392342622836,6.));
#6310=CARTESIAN_POINT('Ctrl Pts',(-8.40527692606173,-2.339459611751,6.));
#6311=CARTESIAN_POINT('Ctrl Pts',(-8.35029826768635,-2.33886640526141,6.));
#6312=CARTESIAN_POINT('Ctrl Pts',(-8.29563322262998,-2.33676998946178,6.));
#6313=CARTESIAN_POINT('Ctrl Pts',(-8.24146380440172,-2.33217339857873,6.));
#6314=CARTESIAN_POINT('Ctrl Pts',(-8.19867202257948,-2.32567282066755,6.));
#6315=CARTESIAN_POINT('Ctrl Pts',(-8.16694940973768,-2.31883955953704,6.));
#6316=CARTESIAN_POINT('Ctrl Pts',(-8.14597432907962,-2.31336634706602,6.));
#6317=CARTESIAN_POINT('Ctrl Pts',(-8.13553012180811,-2.31040030805734,6.));
#6318=CARTESIAN_POINT('',(-11.9792754136349,-0.704954299427494,0.));
#6319=CARTESIAN_POINT('Origin',(-3.99680288865056E-13,3.15544362088405E-29,
0.));
#6320=CARTESIAN_POINT('',(-11.9792754136349,0.70495429942753,-1.));
#6321=CARTESIAN_POINT('Origin',(-3.99680288865056E-13,3.15544362088405E-29,
-1.));
#6322=CARTESIAN_POINT('',(-11.9792754136349,0.70495429942753,6.));
#6323=CARTESIAN_POINT('Origin',(-3.99680288865056E-13,3.15544362088405E-29,
6.));
#6324=CARTESIAN_POINT('',(-11.9792754136349,0.70495429942753,0.));
#6325=CARTESIAN_POINT('Ctrl Pts',(-8.13553012180811,2.31040030805735,-3.75));
#6326=CARTESIAN_POINT('Ctrl Pts',(-8.13553012180811,2.31040030805735,12.75));
#6327=CARTESIAN_POINT('Ctrl Pts',(-8.14597432907962,2.31336634706602,-3.75));
#6328=CARTESIAN_POINT('Ctrl Pts',(-8.14597432907962,2.31336634706602,12.75));
#6329=CARTESIAN_POINT('Ctrl Pts',(-8.16694940973767,2.31883955953704,-3.75));
#6330=CARTESIAN_POINT('Ctrl Pts',(-8.16694940973767,2.31883955953704,12.75));
#6331=CARTESIAN_POINT('Ctrl Pts',(-8.19867202257948,2.32567282066756,-3.75));
#6332=CARTESIAN_POINT('Ctrl Pts',(-8.19867202257948,2.32567282066756,12.75));
#6333=CARTESIAN_POINT('Ctrl Pts',(-8.24146380440172,2.33217339857874,-3.75));
#6334=CARTESIAN_POINT('Ctrl Pts',(-8.24146380440172,2.33217339857874,12.75));
#6335=CARTESIAN_POINT('Ctrl Pts',(-8.29563322262998,2.33676998946179,-3.75));
#6336=CARTESIAN_POINT('Ctrl Pts',(-8.29563322262998,2.33676998946179,12.75));
#6337=CARTESIAN_POINT('Ctrl Pts',(-8.35029826768635,2.33886640526142,-3.75));
#6338=CARTESIAN_POINT('Ctrl Pts',(-8.35029826768635,2.33886640526142,12.75));
#6339=CARTESIAN_POINT('Ctrl Pts',(-8.40527692606173,2.33945961175101,-3.75));
#6340=CARTESIAN_POINT('Ctrl Pts',(-8.40527692606173,2.33945961175101,12.75));
#6341=CARTESIAN_POINT('Ctrl Pts',(-8.46043689627596,2.3392342622836,-3.75));
#6342=CARTESIAN_POINT('Ctrl Pts',(-8.46043689627596,2.3392342622836,12.75));
#6343=CARTESIAN_POINT('Ctrl Pts',(-8.51572283259063,2.33840535058003,-3.75));
#6344=CARTESIAN_POINT('Ctrl Pts',(-8.51572283259063,2.33840535058003,12.75));
#6345=CARTESIAN_POINT('Ctrl Pts',(-8.57112741281372,2.33689888190034,-3.75));
#6346=CARTESIAN_POINT('Ctrl Pts',(-8.57112741281372,2.33689888190034,12.75));
#6347=CARTESIAN_POINT('Ctrl Pts',(-8.62667187892838,2.33447589689188,-3.75));
#6348=CARTESIAN_POINT('Ctrl Pts',(-8.62667187892838,2.33447589689188,12.75));
#6349=CARTESIAN_POINT('Ctrl Pts',(-8.68238458286971,2.33086762045752,-3.75));
#6350=CARTESIAN_POINT('Ctrl Pts',(-8.68238458286971,2.33086762045752,12.75));
#6351=CARTESIAN_POINT('Ctrl Pts',(-8.73827625692193,2.32593252219559,-3.75));
#6352=CARTESIAN_POINT('Ctrl Pts',(-8.73827625692193,2.32593252219559,12.75));
#6353=CARTESIAN_POINT('Ctrl Pts',(-8.79433301721166,2.31969862084206,-3.75));
#6354=CARTESIAN_POINT('Ctrl Pts',(-8.79433301721166,2.31969862084206,12.75));
#6355=CARTESIAN_POINT('Ctrl Pts',(-8.85052793120604,2.31228619203479,-3.75));
#6356=CARTESIAN_POINT('Ctrl Pts',(-8.85052793120604,2.31228619203479,12.75));
#6357=CARTESIAN_POINT('Ctrl Pts',(-8.90682777405608,2.30386137247017,-3.75));
#6358=CARTESIAN_POINT('Ctrl Pts',(-8.90682777405608,2.30386137247017,12.75));
#6359=CARTESIAN_POINT('Ctrl Pts',(-8.96320109950669,2.29458154408801,-3.75));
#6360=CARTESIAN_POINT('Ctrl Pts',(-8.96320109950669,2.29458154408801,12.75));
#6361=CARTESIAN_POINT('Ctrl Pts',(-9.0196273647496,2.28453333318601,-3.75));
#6362=CARTESIAN_POINT('Ctrl Pts',(-9.0196273647496,2.28453333318601,12.75));
#6363=CARTESIAN_POINT('Ctrl Pts',(-9.07609679780011,2.27373321015996,-3.75));
#6364=CARTESIAN_POINT('Ctrl Pts',(-9.07609679780011,2.27373321015996,12.75));
#6365=CARTESIAN_POINT('Ctrl Pts',(-9.13260588645235,2.26215759393014,-3.75));
#6366=CARTESIAN_POINT('Ctrl Pts',(-9.13260588645235,2.26215759393014,12.75));
#6367=CARTESIAN_POINT('Ctrl Pts',(-9.18915420809356,2.24976392906278,-3.75));
#6368=CARTESIAN_POINT('Ctrl Pts',(-9.18915420809356,2.24976392906278,12.75));
#6369=CARTESIAN_POINT('Ctrl Pts',(-9.24574089753053,2.23651421201962,-3.75));
#6370=CARTESIAN_POINT('Ctrl Pts',(-9.24574089753053,2.23651421201962,12.75));
#6371=CARTESIAN_POINT('Ctrl Pts',(-9.30236077039476,2.22240082168223,-3.75));
#6372=CARTESIAN_POINT('Ctrl Pts',(-9.30236077039476,2.22240082168223,12.75));
#6373=CARTESIAN_POINT('Ctrl Pts',(-9.35900502856467,2.2074416540289,-3.75));
#6374=CARTESIAN_POINT('Ctrl Pts',(-9.35900502856467,2.2074416540289,12.75));
#6375=CARTESIAN_POINT('Ctrl Pts',(-9.41566291502215,2.19166889809877,-3.75));
#6376=CARTESIAN_POINT('Ctrl Pts',(-9.41566291502215,2.19166889809877,12.75));
#6377=CARTESIAN_POINT('Ctrl Pts',(-9.4723230488593,2.17511995998945,-3.75));
#6378=CARTESIAN_POINT('Ctrl Pts',(-9.4723230488593,2.17511995998945,12.75));
#6379=CARTESIAN_POINT('Ctrl Pts',(-9.52897485563506,2.15782775391113,-3.75));
#6380=CARTESIAN_POINT('Ctrl Pts',(-9.52897485563506,2.15782775391113,12.75));
#6381=CARTESIAN_POINT('Ctrl Pts',(-9.58561005875903,2.13981058538588,-3.75));
#6382=CARTESIAN_POINT('Ctrl Pts',(-9.58561005875903,2.13981058538588,12.75));
#6383=CARTESIAN_POINT('Ctrl Pts',(-9.64222216484242,2.12107554726937,-3.75));
#6384=CARTESIAN_POINT('Ctrl Pts',(-9.64222216484242,2.12107554726937,12.75));
#6385=CARTESIAN_POINT('Ctrl Pts',(-9.69880579601398,2.10162295100989,-3.75));
#6386=CARTESIAN_POINT('Ctrl Pts',(-9.69880579601398,2.10162295100989,12.75));
#6387=CARTESIAN_POINT('Ctrl Pts',(-9.75535607889872,2.08145038176733,-3.75));
#6388=CARTESIAN_POINT('Ctrl Pts',(-9.75535607889872,2.08145038176733,12.75));
#6389=CARTESIAN_POINT('Ctrl Pts',(-9.81186801391803,2.06055689146528,-3.75));
#6390=CARTESIAN_POINT('Ctrl Pts',(-9.81186801391803,2.06055689146528,12.75));
#6391=CARTESIAN_POINT('Ctrl Pts',(-9.86833584478527,2.03894719582859,-3.75));
#6392=CARTESIAN_POINT('Ctrl Pts',(-9.86833584478527,2.03894719582859,12.75));
#6393=CARTESIAN_POINT('Ctrl Pts',(-9.92475330165988,2.01663001707736,-3.75));
#6394=CARTESIAN_POINT('Ctrl Pts',(-9.92475330165988,2.01663001707736,12.75));
#6395=CARTESIAN_POINT('Ctrl Pts',(-9.98111385659409,1.99361634997092,-3.75));
#6396=CARTESIAN_POINT('Ctrl Pts',(-9.98111385659409,1.99361634997092,12.75));
#6397=CARTESIAN_POINT('Ctrl Pts',(-10.037410974034,1.96991776698621,-3.75));
#6398=CARTESIAN_POINT('Ctrl Pts',(-10.037410974034,1.96991776698621,12.75));
#6399=CARTESIAN_POINT('Ctrl Pts',(-10.0936383641523,1.94554471072257,-3.75));
#6400=CARTESIAN_POINT('Ctrl Pts',(-10.0936383641523,1.94554471072257,12.75));
#6401=CARTESIAN_POINT('Ctrl Pts',(-10.1497902344364,1.92050480406378,-3.75));
#6402=CARTESIAN_POINT('Ctrl Pts',(-10.1497902344364,1.92050480406378,12.75));
#6403=CARTESIAN_POINT('Ctrl Pts',(-10.2058611678956,1.89480360265125,-3.75));
#6404=CARTESIAN_POINT('Ctrl Pts',(-10.2058611678956,1.89480360265125,12.75));
#6405=CARTESIAN_POINT('Ctrl Pts',(-10.2618460035706,1.86844533887956,-3.75));
#6406=CARTESIAN_POINT('Ctrl Pts',(-10.2618460035706,1.86844533887956,12.75));
#6407=CARTESIAN_POINT('Ctrl Pts',(-10.317739716759,1.84143367405763,-3.75));
#6408=CARTESIAN_POINT('Ctrl Pts',(-10.317739716759,1.84143367405763,12.75));
#6409=CARTESIAN_POINT('Ctrl Pts',(-10.3735373011506,1.81377244526719,-3.75));
#6410=CARTESIAN_POINT('Ctrl Pts',(-10.3735373011506,1.81377244526719,12.75));
#6411=CARTESIAN_POINT('Ctrl Pts',(-10.4292336483793,1.78546643461776,-3.75));
#6412=CARTESIAN_POINT('Ctrl Pts',(-10.4292336483793,1.78546643461776,12.75));
#6413=CARTESIAN_POINT('Ctrl Pts',(-10.4848236013528,1.75652107004318,-3.75));
#6414=CARTESIAN_POINT('Ctrl Pts',(-10.4848236013528,1.75652107004318,12.75));
#6415=CARTESIAN_POINT('Ctrl Pts',(-10.5403020105194,1.72694211360793,-3.75));
#6416=CARTESIAN_POINT('Ctrl Pts',(-10.5403020105194,1.72694211360793,12.75));
#6417=CARTESIAN_POINT('Ctrl Pts',(-10.59566379085,1.69673535547185,-3.75));
#6418=CARTESIAN_POINT('Ctrl Pts',(-10.59566379085,1.69673535547185,12.75));
#6419=CARTESIAN_POINT('Ctrl Pts',(-10.6509039769739,1.66590631967585,-3.75));
#6420=CARTESIAN_POINT('Ctrl Pts',(-10.6509039769739,1.66590631967585,12.75));
#6421=CARTESIAN_POINT('Ctrl Pts',(-10.7060177866027,1.63445994423349,-3.75));
#6422=CARTESIAN_POINT('Ctrl Pts',(-10.7060177866027,1.63445994423349,12.75));
#6423=CARTESIAN_POINT('Ctrl Pts',(-10.761000572936,1.60240070038749,-3.75));
#6424=CARTESIAN_POINT('Ctrl Pts',(-10.761000572936,1.60240070038749,12.75));
#6425=CARTESIAN_POINT('Ctrl Pts',(-10.8158477697972,1.56973274862052,-3.75));
#6426=CARTESIAN_POINT('Ctrl Pts',(-10.8158477697972,1.56973274862052,12.75));
#6427=CARTESIAN_POINT('Ctrl Pts',(-10.8705548380775,1.53646008988796,-3.75));
#6428=CARTESIAN_POINT('Ctrl Pts',(-10.8705548380775,1.53646008988796,12.75));
#6429=CARTESIAN_POINT('Ctrl Pts',(-10.9251172180581,1.50258671261028,-3.75));
#6430=CARTESIAN_POINT('Ctrl Pts',(-10.9251172180581,1.50258671261028,12.75));
#6431=CARTESIAN_POINT('Ctrl Pts',(-10.9795302662584,1.46811677324654,-3.75));
#6432=CARTESIAN_POINT('Ctrl Pts',(-10.9795302662584,1.46811677324654,12.75));
#6433=CARTESIAN_POINT('Ctrl Pts',(-11.033789312906,1.43305454241432,-3.75));
#6434=CARTESIAN_POINT('Ctrl Pts',(-11.033789312906,1.43305454241432,12.75));
#6435=CARTESIAN_POINT('Ctrl Pts',(-11.0878897426906,1.39740430473757,-3.75));
#6436=CARTESIAN_POINT('Ctrl Pts',(-11.0878897426906,1.39740430473757,12.75));
#6437=CARTESIAN_POINT('Ctrl Pts',(-11.1418270749817,1.36117027439398,-3.75));
#6438=CARTESIAN_POINT('Ctrl Pts',(-11.1418270749817,1.36117027439398,12.75));
#6439=CARTESIAN_POINT('Ctrl Pts',(-11.1955970312291,1.32435651843207,-3.75));
#6440=CARTESIAN_POINT('Ctrl Pts',(-11.1955970312291,1.32435651843207,12.75));
#6441=CARTESIAN_POINT('Ctrl Pts',(-11.2491956455455,1.28696685552412,-3.75));
#6442=CARTESIAN_POINT('Ctrl Pts',(-11.2491956455455,1.28696685552412,12.75));
#6443=CARTESIAN_POINT('Ctrl Pts',(-11.30261917075,1.24900490126928,-3.75));
#6444=CARTESIAN_POINT('Ctrl Pts',(-11.30261917075,1.24900490126928,12.75));
#6445=CARTESIAN_POINT('Ctrl Pts',(-11.3558638941869,1.21047418192819,-3.75));
#6446=CARTESIAN_POINT('Ctrl Pts',(-11.3558638941869,1.21047418192819,12.75));
#6447=CARTESIAN_POINT('Ctrl Pts',(-11.4089259705106,1.17137823760545,-3.75));
#6448=CARTESIAN_POINT('Ctrl Pts',(-11.4089259705106,1.17137823760545,12.75));
#6449=CARTESIAN_POINT('Ctrl Pts',(-11.4618012771636,1.13172071766774,-3.75));
#6450=CARTESIAN_POINT('Ctrl Pts',(-11.4618012771636,1.13172071766774,12.75));
#6451=CARTESIAN_POINT('Ctrl Pts',(-11.5144851912285,1.09150552381395,-3.75));
#6452=CARTESIAN_POINT('Ctrl Pts',(-11.5144851912285,1.09150552381395,12.75));
#6453=CARTESIAN_POINT('Ctrl Pts',(-11.5669726710206,1.05073678224335,-3.75));
#6454=CARTESIAN_POINT('Ctrl Pts',(-11.5669726710206,1.05073678224335,12.75));
#6455=CARTESIAN_POINT('Ctrl Pts',(-11.6192586585895,1.00941863307588,-3.75));
#6456=CARTESIAN_POINT('Ctrl Pts',(-11.6192586585895,1.00941863307588,12.75));
#6457=CARTESIAN_POINT('Ctrl Pts',(-11.6713384077523,0.967555069553195,-3.75));
#6458=CARTESIAN_POINT('Ctrl Pts',(-11.6713384077523,0.967555069553195,12.75));
#6459=CARTESIAN_POINT('Ctrl Pts',(-11.7232078225909,0.925149766751162,-3.75));
#6460=CARTESIAN_POINT('Ctrl Pts',(-11.7232078225909,0.925149766751162,12.75));
#6461=CARTESIAN_POINT('Ctrl Pts',(-11.7748638454684,0.882205904336898,-3.75));
#6462=CARTESIAN_POINT('Ctrl Pts',(-11.7748638454684,0.882205904336898,12.75));
#6463=CARTESIAN_POINT('Ctrl Pts',(-11.8263046631092,0.838726039995983,-3.75));
#6464=CARTESIAN_POINT('Ctrl Pts',(-11.8263046631092,0.838726039995983,12.75));
#6465=CARTESIAN_POINT('Ctrl Pts',(-11.877529348846,0.794712140666327,-3.75));
#6466=CARTESIAN_POINT('Ctrl Pts',(-11.877529348846,0.794712140666327,12.75));
#6467=CARTESIAN_POINT('Ctrl Pts',(-11.9183359560736,0.759074898533419,-3.75));
#6468=CARTESIAN_POINT('Ctrl Pts',(-11.9183359560736,0.759074898533419,12.75));
#6469=CARTESIAN_POINT('Ctrl Pts',(-11.9488435391885,0.732107639766311,-3.75));
#6470=CARTESIAN_POINT('Ctrl Pts',(-11.9488435391885,0.732107639766311,12.75));
#6471=CARTESIAN_POINT('Ctrl Pts',(-11.9691386658393,0.714023134927412,-3.75));
#6472=CARTESIAN_POINT('Ctrl Pts',(-11.9691386658393,0.714023134927412,12.75));
#6473=CARTESIAN_POINT('Ctrl Pts',(-11.9792754136349,0.70495429942753,-3.75));
#6474=CARTESIAN_POINT('Ctrl Pts',(-11.9792754136349,0.70495429942753,12.75));
#6475=CARTESIAN_POINT('Ctrl Pts',(-8.13553012180811,2.31040030805735,-1.));
#6476=CARTESIAN_POINT('Ctrl Pts',(-8.14597432907962,2.31336634706602,-1.));
#6477=CARTESIAN_POINT('Ctrl Pts',(-8.16694940973767,2.31883955953704,-1.));
#6478=CARTESIAN_POINT('Ctrl Pts',(-8.19867202257948,2.32567282066756,-1.));
#6479=CARTESIAN_POINT('Ctrl Pts',(-8.24146380440172,2.33217339857874,-1.));
#6480=CARTESIAN_POINT('Ctrl Pts',(-8.29563322262998,2.33676998946179,-1.));
#6481=CARTESIAN_POINT('Ctrl Pts',(-8.35029826768635,2.33886640526142,-1.));
#6482=CARTESIAN_POINT('Ctrl Pts',(-8.40527692606173,2.33945961175101,-1.));
#6483=CARTESIAN_POINT('Ctrl Pts',(-8.46043689627596,2.3392342622836,-1.));
#6484=CARTESIAN_POINT('Ctrl Pts',(-8.51572283259063,2.33840535058003,-1.));
#6485=CARTESIAN_POINT('Ctrl Pts',(-8.57112741281372,2.33689888190034,-1.));
#6486=CARTESIAN_POINT('Ctrl Pts',(-8.62667187892838,2.33447589689188,-1.));
#6487=CARTESIAN_POINT('Ctrl Pts',(-8.68238458286971,2.33086762045752,-1.));
#6488=CARTESIAN_POINT('Ctrl Pts',(-8.73827625692193,2.32593252219559,-1.));
#6489=CARTESIAN_POINT('Ctrl Pts',(-8.79433301721166,2.31969862084206,-1.));
#6490=CARTESIAN_POINT('Ctrl Pts',(-8.85052793120604,2.31228619203479,-1.));
#6491=CARTESIAN_POINT('Ctrl Pts',(-8.90682777405608,2.30386137247017,-1.));
#6492=CARTESIAN_POINT('Ctrl Pts',(-8.96320109950669,2.29458154408801,-1.));
#6493=CARTESIAN_POINT('Ctrl Pts',(-9.0196273647496,2.28453333318601,-1.));
#6494=CARTESIAN_POINT('Ctrl Pts',(-9.07609679780011,2.27373321015996,-1.));
#6495=CARTESIAN_POINT('Ctrl Pts',(-9.13260588645235,2.26215759393014,-1.));
#6496=CARTESIAN_POINT('Ctrl Pts',(-9.18915420809356,2.24976392906278,-1.));
#6497=CARTESIAN_POINT('Ctrl Pts',(-9.24574089753053,2.23651421201962,-1.));
#6498=CARTESIAN_POINT('Ctrl Pts',(-9.30236077039476,2.22240082168223,-1.));
#6499=CARTESIAN_POINT('Ctrl Pts',(-9.35900502856467,2.2074416540289,-1.));
#6500=CARTESIAN_POINT('Ctrl Pts',(-9.41566291502215,2.19166889809877,-1.));
#6501=CARTESIAN_POINT('Ctrl Pts',(-9.4723230488593,2.17511995998945,-1.));
#6502=CARTESIAN_POINT('Ctrl Pts',(-9.52897485563506,2.15782775391113,-1.));
#6503=CARTESIAN_POINT('Ctrl Pts',(-9.58561005875903,2.13981058538588,-1.));
#6504=CARTESIAN_POINT('Ctrl Pts',(-9.64222216484242,2.12107554726937,-1.));
#6505=CARTESIAN_POINT('Ctrl Pts',(-9.69880579601398,2.10162295100989,-1.));
#6506=CARTESIAN_POINT('Ctrl Pts',(-9.75535607889872,2.08145038176733,-1.));
#6507=CARTESIAN_POINT('Ctrl Pts',(-9.81186801391803,2.06055689146528,-1.));
#6508=CARTESIAN_POINT('Ctrl Pts',(-9.86833584478527,2.03894719582859,-1.));
#6509=CARTESIAN_POINT('Ctrl Pts',(-9.92475330165988,2.01663001707736,-1.));
#6510=CARTESIAN_POINT('Ctrl Pts',(-9.98111385659409,1.99361634997092,-1.));
#6511=CARTESIAN_POINT('Ctrl Pts',(-10.037410974034,1.96991776698621,-1.));
#6512=CARTESIAN_POINT('Ctrl Pts',(-10.0936383641523,1.94554471072257,-1.));
#6513=CARTESIAN_POINT('Ctrl Pts',(-10.1497902344364,1.92050480406378,-1.));
#6514=CARTESIAN_POINT('Ctrl Pts',(-10.2058611678956,1.89480360265125,-1.));
#6515=CARTESIAN_POINT('Ctrl Pts',(-10.2618460035706,1.86844533887956,-1.));
#6516=CARTESIAN_POINT('Ctrl Pts',(-10.317739716759,1.84143367405763,-1.));
#6517=CARTESIAN_POINT('Ctrl Pts',(-10.3735373011506,1.81377244526719,-1.));
#6518=CARTESIAN_POINT('Ctrl Pts',(-10.4292336483793,1.78546643461776,-1.));
#6519=CARTESIAN_POINT('Ctrl Pts',(-10.4848236013528,1.75652107004318,-1.));
#6520=CARTESIAN_POINT('Ctrl Pts',(-10.5403020105194,1.72694211360793,-1.));
#6521=CARTESIAN_POINT('Ctrl Pts',(-10.59566379085,1.69673535547185,-1.));
#6522=CARTESIAN_POINT('Ctrl Pts',(-10.6509039769739,1.66590631967585,-1.));
#6523=CARTESIAN_POINT('Ctrl Pts',(-10.7060177866027,1.63445994423349,-1.));
#6524=CARTESIAN_POINT('Ctrl Pts',(-10.761000572936,1.60240070038749,-1.));
#6525=CARTESIAN_POINT('Ctrl Pts',(-10.8158477697972,1.56973274862052,-1.));
#6526=CARTESIAN_POINT('Ctrl Pts',(-10.8705548380775,1.53646008988796,-1.));
#6527=CARTESIAN_POINT('Ctrl Pts',(-10.9251172180581,1.50258671261028,-1.));
#6528=CARTESIAN_POINT('Ctrl Pts',(-10.9795302662584,1.46811677324654,-1.));
#6529=CARTESIAN_POINT('Ctrl Pts',(-11.033789312906,1.43305454241432,-1.));
#6530=CARTESIAN_POINT('Ctrl Pts',(-11.0878897426906,1.39740430473757,-1.));
#6531=CARTESIAN_POINT('Ctrl Pts',(-11.1418270749817,1.36117027439398,-1.));
#6532=CARTESIAN_POINT('Ctrl Pts',(-11.1955970312291,1.32435651843207,-1.));
#6533=CARTESIAN_POINT('Ctrl Pts',(-11.2491956455455,1.28696685552412,-1.));
#6534=CARTESIAN_POINT('Ctrl Pts',(-11.30261917075,1.24900490126928,-1.));
#6535=CARTESIAN_POINT('Ctrl Pts',(-11.3558638941869,1.21047418192819,-1.));
#6536=CARTESIAN_POINT('Ctrl Pts',(-11.4089259705106,1.17137823760545,-1.));
#6537=CARTESIAN_POINT('Ctrl Pts',(-11.4618012771636,1.13172071766774,-1.));
#6538=CARTESIAN_POINT('Ctrl Pts',(-11.5144851912285,1.09150552381395,-1.));
#6539=CARTESIAN_POINT('Ctrl Pts',(-11.5669726710206,1.05073678224335,-1.));
#6540=CARTESIAN_POINT('Ctrl Pts',(-11.6192586585895,1.00941863307588,-1.));
#6541=CARTESIAN_POINT('Ctrl Pts',(-11.6713384077523,0.967555069553195,-1.));
#6542=CARTESIAN_POINT('Ctrl Pts',(-11.7232078225909,0.925149766751162,-1.));
#6543=CARTESIAN_POINT('Ctrl Pts',(-11.7748638454684,0.882205904336898,-1.));
#6544=CARTESIAN_POINT('Ctrl Pts',(-11.8263046631092,0.838726039995983,-1.));
#6545=CARTESIAN_POINT('Ctrl Pts',(-11.877529348846,0.794712140666327,-1.));
#6546=CARTESIAN_POINT('Ctrl Pts',(-11.9183359560736,0.759074898533419,-1.));
#6547=CARTESIAN_POINT('Ctrl Pts',(-11.9488435391885,0.732107639766311,-1.));
#6548=CARTESIAN_POINT('Ctrl Pts',(-11.9691386658393,0.714023134927412,-1.));
#6549=CARTESIAN_POINT('Ctrl Pts',(-11.9792754136349,0.70495429942753,-1.));
#6550=CARTESIAN_POINT('Ctrl Pts',(-8.13553012180811,2.31040030805735,6.));
#6551=CARTESIAN_POINT('Ctrl Pts',(-8.14597432907962,2.31336634706602,6.));
#6552=CARTESIAN_POINT('Ctrl Pts',(-8.16694940973767,2.31883955953704,6.));
#6553=CARTESIAN_POINT('Ctrl Pts',(-8.19867202257948,2.32567282066756,6.));
#6554=CARTESIAN_POINT('Ctrl Pts',(-8.24146380440172,2.33217339857874,6.));
#6555=CARTESIAN_POINT('Ctrl Pts',(-8.29563322262998,2.33676998946179,6.));
#6556=CARTESIAN_POINT('Ctrl Pts',(-8.35029826768635,2.33886640526142,6.));
#6557=CARTESIAN_POINT('Ctrl Pts',(-8.40527692606173,2.33945961175101,6.));
#6558=CARTESIAN_POINT('Ctrl Pts',(-8.46043689627596,2.3392342622836,6.));
#6559=CARTESIAN_POINT('Ctrl Pts',(-8.51572283259063,2.33840535058003,6.));
#6560=CARTESIAN_POINT('Ctrl Pts',(-8.57112741281372,2.33689888190034,6.));
#6561=CARTESIAN_POINT('Ctrl Pts',(-8.62667187892838,2.33447589689188,6.));
#6562=CARTESIAN_POINT('Ctrl Pts',(-8.68238458286971,2.33086762045752,6.));
#6563=CARTESIAN_POINT('Ctrl Pts',(-8.73827625692193,2.32593252219559,6.));
#6564=CARTESIAN_POINT('Ctrl Pts',(-8.79433301721166,2.31969862084206,6.));
#6565=CARTESIAN_POINT('Ctrl Pts',(-8.85052793120604,2.31228619203479,6.));
#6566=CARTESIAN_POINT('Ctrl Pts',(-8.90682777405608,2.30386137247017,6.));
#6567=CARTESIAN_POINT('Ctrl Pts',(-8.96320109950669,2.29458154408801,6.));
#6568=CARTESIAN_POINT('Ctrl Pts',(-9.0196273647496,2.28453333318601,6.));
#6569=CARTESIAN_POINT('Ctrl Pts',(-9.07609679780011,2.27373321015996,6.));
#6570=CARTESIAN_POINT('Ctrl Pts',(-9.13260588645235,2.26215759393014,6.));
#6571=CARTESIAN_POINT('Ctrl Pts',(-9.18915420809356,2.24976392906278,6.));
#6572=CARTESIAN_POINT('Ctrl Pts',(-9.24574089753053,2.23651421201962,6.));
#6573=CARTESIAN_POINT('Ctrl Pts',(-9.30236077039476,2.22240082168223,6.));
#6574=CARTESIAN_POINT('Ctrl Pts',(-9.35900502856467,2.2074416540289,6.));
#6575=CARTESIAN_POINT('Ctrl Pts',(-9.41566291502215,2.19166889809877,6.));
#6576=CARTESIAN_POINT('Ctrl Pts',(-9.4723230488593,2.17511995998945,6.));
#6577=CARTESIAN_POINT('Ctrl Pts',(-9.52897485563506,2.15782775391113,6.));
#6578=CARTESIAN_POINT('Ctrl Pts',(-9.58561005875903,2.13981058538588,6.));
#6579=CARTESIAN_POINT('Ctrl Pts',(-9.64222216484242,2.12107554726937,6.));
#6580=CARTESIAN_POINT('Ctrl Pts',(-9.69880579601398,2.10162295100989,6.));
#6581=CARTESIAN_POINT('Ctrl Pts',(-9.75535607889872,2.08145038176733,6.));
#6582=CARTESIAN_POINT('Ctrl Pts',(-9.81186801391803,2.06055689146528,6.));
#6583=CARTESIAN_POINT('Ctrl Pts',(-9.86833584478527,2.03894719582859,6.));
#6584=CARTESIAN_POINT('Ctrl Pts',(-9.92475330165988,2.01663001707736,6.));
#6585=CARTESIAN_POINT('Ctrl Pts',(-9.98111385659409,1.99361634997092,6.));
#6586=CARTESIAN_POINT('Ctrl Pts',(-10.037410974034,1.96991776698621,6.));
#6587=CARTESIAN_POINT('Ctrl Pts',(-10.0936383641523,1.94554471072257,6.));
#6588=CARTESIAN_POINT('Ctrl Pts',(-10.1497902344364,1.92050480406378,6.));
#6589=CARTESIAN_POINT('Ctrl Pts',(-10.2058611678956,1.89480360265125,6.));
#6590=CARTESIAN_POINT('Ctrl Pts',(-10.2618460035706,1.86844533887956,6.));
#6591=CARTESIAN_POINT('Ctrl Pts',(-10.317739716759,1.84143367405763,6.));
#6592=CARTESIAN_POINT('Ctrl Pts',(-10.3735373011506,1.81377244526719,6.));
#6593=CARTESIAN_POINT('Ctrl Pts',(-10.4292336483793,1.78546643461776,6.));
#6594=CARTESIAN_POINT('Ctrl Pts',(-10.4848236013528,1.75652107004318,6.));
#6595=CARTESIAN_POINT('Ctrl Pts',(-10.5403020105194,1.72694211360793,6.));
#6596=CARTESIAN_POINT('Ctrl Pts',(-10.59566379085,1.69673535547185,6.));
#6597=CARTESIAN_POINT('Ctrl Pts',(-10.6509039769739,1.66590631967585,6.));
#6598=CARTESIAN_POINT('Ctrl Pts',(-10.7060177866027,1.63445994423349,6.));
#6599=CARTESIAN_POINT('Ctrl Pts',(-10.761000572936,1.60240070038749,6.));
#6600=CARTESIAN_POINT('Ctrl Pts',(-10.8158477697972,1.56973274862052,6.));
#6601=CARTESIAN_POINT('Ctrl Pts',(-10.8705548380775,1.53646008988796,6.));
#6602=CARTESIAN_POINT('Ctrl Pts',(-10.9251172180581,1.50258671261028,6.));
#6603=CARTESIAN_POINT('Ctrl Pts',(-10.9795302662584,1.46811677324654,6.));
#6604=CARTESIAN_POINT('Ctrl Pts',(-11.033789312906,1.43305454241432,6.));
#6605=CARTESIAN_POINT('Ctrl Pts',(-11.0878897426906,1.39740430473757,6.));
#6606=CARTESIAN_POINT('Ctrl Pts',(-11.1418270749817,1.36117027439398,6.));
#6607=CARTESIAN_POINT('Ctrl Pts',(-11.1955970312291,1.32435651843207,6.));
#6608=CARTESIAN_POINT('Ctrl Pts',(-11.2491956455455,1.28696685552412,6.));
#6609=CARTESIAN_POINT('Ctrl Pts',(-11.30261917075,1.24900490126928,6.));
#6610=CARTESIAN_POINT('Ctrl Pts',(-11.3558638941869,1.21047418192819,6.));
#6611=CARTESIAN_POINT('Ctrl Pts',(-11.4089259705106,1.17137823760545,6.));
#6612=CARTESIAN_POINT('Ctrl Pts',(-11.4618012771636,1.13172071766774,6.));
#6613=CARTESIAN_POINT('Ctrl Pts',(-11.5144851912285,1.09150552381395,6.));
#6614=CARTESIAN_POINT('Ctrl Pts',(-11.5669726710206,1.05073678224335,6.));
#6615=CARTESIAN_POINT('Ctrl Pts',(-11.6192586585895,1.00941863307588,6.));
#6616=CARTESIAN_POINT('Ctrl Pts',(-11.6713384077523,0.967555069553195,6.));
#6617=CARTESIAN_POINT('Ctrl Pts',(-11.7232078225909,0.925149766751162,6.));
#6618=CARTESIAN_POINT('Ctrl Pts',(-11.7748638454684,0.882205904336898,6.));
#6619=CARTESIAN_POINT('Ctrl Pts',(-11.8263046631092,0.838726039995983,6.));
#6620=CARTESIAN_POINT('Ctrl Pts',(-11.877529348846,0.794712140666327,6.));
#6621=CARTESIAN_POINT('Ctrl Pts',(-11.9183359560736,0.759074898533419,6.));
#6622=CARTESIAN_POINT('Ctrl Pts',(-11.9488435391885,0.732107639766311,6.));
#6623=CARTESIAN_POINT('Ctrl Pts',(-11.9691386658393,0.714023134927412,6.));
#6624=CARTESIAN_POINT('Ctrl Pts',(-11.9792754136349,0.70495429942753,6.));
#6625=CARTESIAN_POINT('Ctrl Pts',(-6.60014603862877,10.0218796774244,-3.75));
#6626=CARTESIAN_POINT('Ctrl Pts',(-6.60014603862877,10.0218796774244,12.75));
#6627=CARTESIAN_POINT('Ctrl Pts',(-6.60293150665659,10.0085665785717,-3.75));
#6628=CARTESIAN_POINT('Ctrl Pts',(-6.60293150665659,10.0085665785717,12.75));
#6629=CARTESIAN_POINT('Ctrl Pts',(-6.60844558393656,9.98194823089968,-3.75));
#6630=CARTESIAN_POINT('Ctrl Pts',(-6.60844558393656,9.98194823089968,12.75));
#6631=CARTESIAN_POINT('Ctrl Pts',(-6.61654612354183,9.94204425953052,-3.75));
#6632=CARTESIAN_POINT('Ctrl Pts',(-6.61654612354183,9.94204425953052,12.75));
#6633=CARTESIAN_POINT('Ctrl Pts',(-6.62700557693596,9.88888607996273,-3.75));
#6634=CARTESIAN_POINT('Ctrl Pts',(-6.62700557693596,9.88888607996273,12.75));
#6635=CARTESIAN_POINT('Ctrl Pts',(-6.63951038900666,9.82251725114898,-3.75));
#6636=CARTESIAN_POINT('Ctrl Pts',(-6.63951038900666,9.82251725114898,12.75));
#6637=CARTESIAN_POINT('Ctrl Pts',(-6.65144464725859,9.75622826411013,-3.75));
#6638=CARTESIAN_POINT('Ctrl Pts',(-6.65144464725859,9.75622826411013,12.75));
#6639=CARTESIAN_POINT('Ctrl Pts',(-6.66280711160719,9.69002090483258,-3.75));
#6640=CARTESIAN_POINT('Ctrl Pts',(-6.66280711160719,9.69002090483258,12.75));
#6641=CARTESIAN_POINT('Ctrl Pts',(-6.67359647366961,9.62389802250188,-3.75));
#6642=CARTESIAN_POINT('Ctrl Pts',(-6.67359647366961,9.62389802250188,12.75));
#6643=CARTESIAN_POINT('Ctrl Pts',(-6.68381150859182,9.55786385494286,-3.75));
#6644=CARTESIAN_POINT('Ctrl Pts',(-6.68381150859182,9.55786385494286,12.75));
#6645=CARTESIAN_POINT('Ctrl Pts',(-6.69345108162377,9.49192378686253,-3.75));
#6646=CARTESIAN_POINT('Ctrl Pts',(-6.69345108162377,9.49192378686253,12.75));
#6647=CARTESIAN_POINT('Ctrl Pts',(-6.70251410760819,9.42608392519667,-3.75));
#6648=CARTESIAN_POINT('Ctrl Pts',(-6.70251410760819,9.42608392519667,12.75));
#6649=CARTESIAN_POINT('Ctrl Pts',(-6.71099953007123,9.36035072031876,-3.75));
#6650=CARTESIAN_POINT('Ctrl Pts',(-6.71099953007123,9.36035072031876,12.75));
#6651=CARTESIAN_POINT('Ctrl Pts',(-6.71890629646186,9.2947306015555,-3.75));
#6652=CARTESIAN_POINT('Ctrl Pts',(-6.71890629646186,9.2947306015555,12.75));
#6653=CARTESIAN_POINT('Ctrl Pts',(-6.72623333926845,9.22922952332026,-3.75));
#6654=CARTESIAN_POINT('Ctrl Pts',(-6.72623333926845,9.22922952332026,12.75));
#6655=CARTESIAN_POINT('Ctrl Pts',(-6.73297955932547,9.16385288053588,-3.75));
#6656=CARTESIAN_POINT('Ctrl Pts',(-6.73297955932547,9.16385288053588,12.75));
#6657=CARTESIAN_POINT('Ctrl Pts',(-6.73914381348523,9.09860577342166,-3.75));
#6658=CARTESIAN_POINT('Ctrl Pts',(-6.73914381348523,9.09860577342166,12.75));
#6659=CARTESIAN_POINT('Ctrl Pts',(-6.74472490424422,9.03349318036199,-3.75));
#6660=CARTESIAN_POINT('Ctrl Pts',(-6.74472490424422,9.03349318036199,12.75));
#6661=CARTESIAN_POINT('Ctrl Pts',(-6.74972157399229,8.96852015431046,-3.75));
#6662=CARTESIAN_POINT('Ctrl Pts',(-6.74972157399229,8.96852015431046,12.75));
#6663=CARTESIAN_POINT('Ctrl Pts',(-6.75413249860576,8.90369203916218,-3.75));
#6664=CARTESIAN_POINT('Ctrl Pts',(-6.75413249860576,8.90369203916218,12.75));
#6665=CARTESIAN_POINT('Ctrl Pts',(-6.75795629519249,8.83901457377471,-3.75));
#6666=CARTESIAN_POINT('Ctrl Pts',(-6.75795629519249,8.83901457377471,12.75));
#6667=CARTESIAN_POINT('Ctrl Pts',(-6.76119155448275,8.77449374557664,-3.75));
#6668=CARTESIAN_POINT('Ctrl Pts',(-6.76119155448275,8.77449374557664,12.75));
#6669=CARTESIAN_POINT('Ctrl Pts',(-6.76383687353852,8.71013569385599,-3.75));
#6670=CARTESIAN_POINT('Ctrl Pts',(-6.76383687353852,8.71013569385599,12.75));
#6671=CARTESIAN_POINT('Ctrl Pts',(-6.76589088878265,8.64594659806298,-3.75));
#6672=CARTESIAN_POINT('Ctrl Pts',(-6.76589088878265,8.64594659806298,12.75));
#6673=CARTESIAN_POINT('Ctrl Pts',(-6.76735232235634,8.5819325577994,-3.75));
#6674=CARTESIAN_POINT('Ctrl Pts',(-6.76735232235634,8.5819325577994,12.75));
#6675=CARTESIAN_POINT('Ctrl Pts',(-6.76822000004555,8.51809951610774,-3.75));
#6676=CARTESIAN_POINT('Ctrl Pts',(-6.76822000004555,8.51809951610774,12.75));
#6677=CARTESIAN_POINT('Ctrl Pts',(-6.76849272647565,8.45445340444926,-3.75));
#6678=CARTESIAN_POINT('Ctrl Pts',(-6.76849272647565,8.45445340444926,12.75));
#6679=CARTESIAN_POINT('Ctrl Pts',(-6.76816918165128,8.39100025749018,-3.75));
#6680=CARTESIAN_POINT('Ctrl Pts',(-6.76816918165128,8.39100025749018,12.75));
#6681=CARTESIAN_POINT('Ctrl Pts',(-6.76724781676282,8.32774633509908,-3.75));
#6682=CARTESIAN_POINT('Ctrl Pts',(-6.76724781676282,8.32774633509908,12.75));
#6683=CARTESIAN_POINT('Ctrl Pts',(-6.76572674650935,8.26469824786603,-3.75));
#6684=CARTESIAN_POINT('Ctrl Pts',(-6.76572674650935,8.26469824786603,12.75));
#6685=CARTESIAN_POINT('Ctrl Pts',(-6.7636036696164,8.20186305794855,-3.75));
#6686=CARTESIAN_POINT('Ctrl Pts',(-6.7636036696164,8.20186305794855,12.75));
#6687=CARTESIAN_POINT('Ctrl Pts',(-6.76087611417306,8.13924806419107,-3.75));
#6688=CARTESIAN_POINT('Ctrl Pts',(-6.76087611417306,8.13924806419107,12.75));
#6689=CARTESIAN_POINT('Ctrl Pts',(-6.75754166486089,8.07686060726828,-3.75));
#6690=CARTESIAN_POINT('Ctrl Pts',(-6.75754166486089,8.07686060726828,12.75));
#6691=CARTESIAN_POINT('Ctrl Pts',(-6.75359819949754,8.01470786732019,-3.75));
#6692=CARTESIAN_POINT('Ctrl Pts',(-6.75359819949754,8.01470786732019,12.75));
#6693=CARTESIAN_POINT('Ctrl Pts',(-6.7490441308376,7.95279665937614,-3.75));
#6694=CARTESIAN_POINT('Ctrl Pts',(-6.7490441308376,7.95279665937614,12.75));
#6695=CARTESIAN_POINT('Ctrl Pts',(-6.74387863902608,7.89113323756913,-3.75));
#6696=CARTESIAN_POINT('Ctrl Pts',(-6.74387863902608,7.89113323756913,12.75));
#6697=CARTESIAN_POINT('Ctrl Pts',(-6.73810106562748,7.82972378407324,-3.75));
#6698=CARTESIAN_POINT('Ctrl Pts',(-6.73810106562748,7.82972378407324,12.75));
#6699=CARTESIAN_POINT('Ctrl Pts',(-6.73171032576035,7.76857488460784,-3.75));
#6700=CARTESIAN_POINT('Ctrl Pts',(-6.73171032576035,7.76857488460784,12.75));
#6701=CARTESIAN_POINT('Ctrl Pts',(-6.72470431659336,7.70769400824503,-3.75));
#6702=CARTESIAN_POINT('Ctrl Pts',(-6.72470431659336,7.70769400824503,12.75));
#6703=CARTESIAN_POINT('Ctrl Pts',(-6.71707933277187,7.6470899828899,-3.75));
#6704=CARTESIAN_POINT('Ctrl Pts',(-6.71707933277187,7.6470899828899,12.75));
#6705=CARTESIAN_POINT('Ctrl Pts',(-6.70882947565318,7.58677347699226,-3.75));
#6706=CARTESIAN_POINT('Ctrl Pts',(-6.70882947565318,7.58677347699226,12.75));
#6707=CARTESIAN_POINT('Ctrl Pts',(-6.69994799095524,7.52675593674632,-3.75));
#6708=CARTESIAN_POINT('Ctrl Pts',(-6.69994799095524,7.52675593674632,12.75));
#6709=CARTESIAN_POINT('Ctrl Pts',(-6.69042862091104,7.46704851290034,-3.75));
#6710=CARTESIAN_POINT('Ctrl Pts',(-6.69042862091104,7.46704851290034,12.75));
#6711=CARTESIAN_POINT('Ctrl Pts',(-6.68026694677668,7.40766099640558,-3.75));
#6712=CARTESIAN_POINT('Ctrl Pts',(-6.68026694677668,7.40766099640558,12.75));
#6713=CARTESIAN_POINT('Ctrl Pts',(-6.66946176275797,7.34860073021492,-3.75));
#6714=CARTESIAN_POINT('Ctrl Pts',(-6.66946176275797,7.34860073021492,12.75));
#6715=CARTESIAN_POINT('Ctrl Pts',(-6.65801638970246,7.28987157005224,-3.75));
#6716=CARTESIAN_POINT('Ctrl Pts',(-6.65801638970246,7.28987157005224,12.75));
#6717=CARTESIAN_POINT('Ctrl Pts',(-6.64593535561053,7.23147652896403,-3.75));
#6718=CARTESIAN_POINT('Ctrl Pts',(-6.64593535561053,7.23147652896403,12.75));
#6719=CARTESIAN_POINT('Ctrl Pts',(-6.63322107969569,7.17342042004756,-3.75));
#6720=CARTESIAN_POINT('Ctrl Pts',(-6.63322107969569,7.17342042004756,12.75));
#6721=CARTESIAN_POINT('Ctrl Pts',(-6.6198706660591,7.1157124131703,-3.75));
#6722=CARTESIAN_POINT('Ctrl Pts',(-6.6198706660591,7.1157124131703,12.75));
#6723=CARTESIAN_POINT('Ctrl Pts',(-6.60587239994885,7.05836882883084,-3.75));
#6724=CARTESIAN_POINT('Ctrl Pts',(-6.60587239994885,7.05836882883084,12.75));
#6725=CARTESIAN_POINT('Ctrl Pts',(-6.5912030640433,7.00141528186886,-3.75));
#6726=CARTESIAN_POINT('Ctrl Pts',(-6.5912030640433,7.00141528186886,12.75));
#6727=CARTESIAN_POINT('Ctrl Pts',(-6.5758359541656,6.94488033148854,-3.75));
#6728=CARTESIAN_POINT('Ctrl Pts',(-6.5758359541656,6.94488033148854,12.75));
#6729=CARTESIAN_POINT('Ctrl Pts',(-6.55974857229919,6.88878938806037,-3.75));
#6730=CARTESIAN_POINT('Ctrl Pts',(-6.55974857229919,6.88878938806037,12.75));
#6731=CARTESIAN_POINT('Ctrl Pts',(-6.54292981913304,6.83315901897031,-3.75));
#6732=CARTESIAN_POINT('Ctrl Pts',(-6.54292981913304,6.83315901897031,12.75));
#6733=CARTESIAN_POINT('Ctrl Pts',(-6.52538888693355,6.77798990345397,-3.75));
#6734=CARTESIAN_POINT('Ctrl Pts',(-6.52538888693355,6.77798990345397,12.75));
#6735=CARTESIAN_POINT('Ctrl Pts',(-6.50715912032692,6.72326378902152,-3.75));
#6736=CARTESIAN_POINT('Ctrl Pts',(-6.50715912032692,6.72326378902152,12.75));
#6737=CARTESIAN_POINT('Ctrl Pts',(-6.48827758470622,6.66895976394944,-3.75));
#6738=CARTESIAN_POINT('Ctrl Pts',(-6.48827758470622,6.66895976394944,12.75));
#6739=CARTESIAN_POINT('Ctrl Pts',(-6.46876645798849,6.6150690793574,-3.75));
#6740=CARTESIAN_POINT('Ctrl Pts',(-6.46876645798849,6.6150690793574,12.75));
#6741=CARTESIAN_POINT('Ctrl Pts',(-6.44861636238489,6.56160843323028,-3.75));
#6742=CARTESIAN_POINT('Ctrl Pts',(-6.44861636238489,6.56160843323028,12.75));
#6743=CARTESIAN_POINT('Ctrl Pts',(-6.42776254872513,6.50863892931077,-3.75));
#6744=CARTESIAN_POINT('Ctrl Pts',(-6.42776254872513,6.50863892931077,12.75));
#6745=CARTESIAN_POINT('Ctrl Pts',(-6.40608444337878,6.45626649182453,-3.75));
#6746=CARTESIAN_POINT('Ctrl Pts',(-6.40608444337878,6.45626649182453,12.75));
#6747=CARTESIAN_POINT('Ctrl Pts',(-6.38345478017075,6.404602962683,-3.75));
#6748=CARTESIAN_POINT('Ctrl Pts',(-6.38345478017075,6.404602962683,12.75));
#6749=CARTESIAN_POINT('Ctrl Pts',(-6.35978286360965,6.35373180396277,-3.75));
#6750=CARTESIAN_POINT('Ctrl Pts',(-6.35978286360965,6.35373180396277,12.75));
#6751=CARTESIAN_POINT('Ctrl Pts',(-6.33505137069502,6.30367904881887,-3.75));
#6752=CARTESIAN_POINT('Ctrl Pts',(-6.33505137069502,6.30367904881887,12.75));
#6753=CARTESIAN_POINT('Ctrl Pts',(-6.30937750420801,6.2543646376197,-3.75));
#6754=CARTESIAN_POINT('Ctrl Pts',(-6.30937750420801,6.2543646376197,12.75));
#6755=CARTESIAN_POINT('Ctrl Pts',(-6.28297985424307,6.20562962932065,-3.75));
#6756=CARTESIAN_POINT('Ctrl Pts',(-6.28297985424307,6.20562962932065,12.75));
#6757=CARTESIAN_POINT('Ctrl Pts',(-6.25605474467853,6.15733614814836,-3.75));
#6758=CARTESIAN_POINT('Ctrl Pts',(-6.25605474467853,6.15733614814836,12.75));
#6759=CARTESIAN_POINT('Ctrl Pts',(-6.22866991793491,6.10945353793714,-3.75));
#6760=CARTESIAN_POINT('Ctrl Pts',(-6.22866991793491,6.10945353793714,12.75));
#6761=CARTESIAN_POINT('Ctrl Pts',(-6.20066685685755,6.06213722636286,-3.75));
#6762=CARTESIAN_POINT('Ctrl Pts',(-6.20066685685755,6.06213722636286,12.75));
#6763=CARTESIAN_POINT('Ctrl Pts',(-6.17151878498999,6.01584411654484,-3.75));
#6764=CARTESIAN_POINT('Ctrl Pts',(-6.17151878498999,6.01584411654484,12.75));
#6765=CARTESIAN_POINT('Ctrl Pts',(-6.14045331140033,5.97123031969247,-3.75));
#6766=CARTESIAN_POINT('Ctrl Pts',(-6.14045331140033,5.97123031969247,12.75));
#6767=CARTESIAN_POINT('Ctrl Pts',(-6.11342775487885,5.9374218385168,-3.75));
#6768=CARTESIAN_POINT('Ctrl Pts',(-6.11342775487885,5.9374218385168,12.75));
#6769=CARTESIAN_POINT('Ctrl Pts',(-6.09164867072823,5.91336588048663,-3.75));
#6770=CARTESIAN_POINT('Ctrl Pts',(-6.09164867072823,5.91336588048663,12.75));
#6771=CARTESIAN_POINT('Ctrl Pts',(-6.07642118935899,5.89793753402585,-3.75));
#6772=CARTESIAN_POINT('Ctrl Pts',(-6.07642118935899,5.89793753402585,12.75));
#6773=CARTESIAN_POINT('Ctrl Pts',(-6.06863042059311,5.89037560471066,-3.75));
#6774=CARTESIAN_POINT('Ctrl Pts',(-6.06863042059311,5.89037560471066,12.75));
#6775=CARTESIAN_POINT('',(-6.60014603862874,10.0218796774245,-1.));
#6776=CARTESIAN_POINT('Ctrl Pts',(-6.60014603862877,10.0218796774244,-1.));
#6777=CARTESIAN_POINT('Ctrl Pts',(-6.60293150665659,10.0085665785717,-1.));
#6778=CARTESIAN_POINT('Ctrl Pts',(-6.60844558393656,9.98194823089968,-1.));
#6779=CARTESIAN_POINT('Ctrl Pts',(-6.61654612354183,9.94204425953052,-1.));
#6780=CARTESIAN_POINT('Ctrl Pts',(-6.62700557693596,9.88888607996273,-1.));
#6781=CARTESIAN_POINT('Ctrl Pts',(-6.63951038900666,9.82251725114898,-1.));
#6782=CARTESIAN_POINT('Ctrl Pts',(-6.65144464725859,9.75622826411013,-1.));
#6783=CARTESIAN_POINT('Ctrl Pts',(-6.66280711160719,9.69002090483258,-1.));
#6784=CARTESIAN_POINT('Ctrl Pts',(-6.67359647366961,9.62389802250188,-1.));
#6785=CARTESIAN_POINT('Ctrl Pts',(-6.68381150859182,9.55786385494286,-1.));
#6786=CARTESIAN_POINT('Ctrl Pts',(-6.69345108162377,9.49192378686253,-1.));
#6787=CARTESIAN_POINT('Ctrl Pts',(-6.70251410760819,9.42608392519667,-1.));
#6788=CARTESIAN_POINT('Ctrl Pts',(-6.71099953007123,9.36035072031876,-1.));
#6789=CARTESIAN_POINT('Ctrl Pts',(-6.71890629646186,9.2947306015555,-1.));
#6790=CARTESIAN_POINT('Ctrl Pts',(-6.72623333926845,9.22922952332026,-1.));
#6791=CARTESIAN_POINT('Ctrl Pts',(-6.73297955932547,9.16385288053588,-1.));
#6792=CARTESIAN_POINT('Ctrl Pts',(-6.73914381348523,9.09860577342166,-1.));
#6793=CARTESIAN_POINT('Ctrl Pts',(-6.74472490424422,9.03349318036199,-1.));
#6794=CARTESIAN_POINT('Ctrl Pts',(-6.74972157399229,8.96852015431046,-1.));
#6795=CARTESIAN_POINT('Ctrl Pts',(-6.75413249860576,8.90369203916218,-1.));
#6796=CARTESIAN_POINT('Ctrl Pts',(-6.75795629519249,8.83901457377471,-1.));
#6797=CARTESIAN_POINT('Ctrl Pts',(-6.76119155448275,8.77449374557664,-1.));
#6798=CARTESIAN_POINT('Ctrl Pts',(-6.76383687353852,8.71013569385599,-1.));
#6799=CARTESIAN_POINT('Ctrl Pts',(-6.76589088878265,8.64594659806298,-1.));
#6800=CARTESIAN_POINT('Ctrl Pts',(-6.76735232235634,8.5819325577994,-1.));
#6801=CARTESIAN_POINT('Ctrl Pts',(-6.76822000004555,8.51809951610774,-1.));
#6802=CARTESIAN_POINT('Ctrl Pts',(-6.76849272647565,8.45445340444926,-1.));
#6803=CARTESIAN_POINT('Ctrl Pts',(-6.76816918165128,8.39100025749018,-1.));
#6804=CARTESIAN_POINT('Ctrl Pts',(-6.76724781676282,8.32774633509908,-1.));
#6805=CARTESIAN_POINT('Ctrl Pts',(-6.76572674650935,8.26469824786603,-1.));
#6806=CARTESIAN_POINT('Ctrl Pts',(-6.7636036696164,8.20186305794855,-1.));
#6807=CARTESIAN_POINT('Ctrl Pts',(-6.76087611417306,8.13924806419107,-1.));
#6808=CARTESIAN_POINT('Ctrl Pts',(-6.75754166486089,8.07686060726828,-1.));
#6809=CARTESIAN_POINT('Ctrl Pts',(-6.75359819949754,8.01470786732019,-1.));
#6810=CARTESIAN_POINT('Ctrl Pts',(-6.7490441308376,7.95279665937614,-1.));
#6811=CARTESIAN_POINT('Ctrl Pts',(-6.74387863902608,7.89113323756913,-1.));
#6812=CARTESIAN_POINT('Ctrl Pts',(-6.73810106562748,7.82972378407324,-1.));
#6813=CARTESIAN_POINT('Ctrl Pts',(-6.73171032576035,7.76857488460784,-1.));
#6814=CARTESIAN_POINT('Ctrl Pts',(-6.72470431659336,7.70769400824503,-1.));
#6815=CARTESIAN_POINT('Ctrl Pts',(-6.71707933277187,7.6470899828899,-1.));
#6816=CARTESIAN_POINT('Ctrl Pts',(-6.70882947565318,7.58677347699226,-1.));
#6817=CARTESIAN_POINT('Ctrl Pts',(-6.69994799095524,7.52675593674632,-1.));
#6818=CARTESIAN_POINT('Ctrl Pts',(-6.69042862091104,7.46704851290034,-1.));
#6819=CARTESIAN_POINT('Ctrl Pts',(-6.68026694677668,7.40766099640558,-1.));
#6820=CARTESIAN_POINT('Ctrl Pts',(-6.66946176275797,7.34860073021492,-1.));
#6821=CARTESIAN_POINT('Ctrl Pts',(-6.65801638970246,7.28987157005224,-1.));
#6822=CARTESIAN_POINT('Ctrl Pts',(-6.64593535561053,7.23147652896403,-1.));
#6823=CARTESIAN_POINT('Ctrl Pts',(-6.63322107969569,7.17342042004756,-1.));
#6824=CARTESIAN_POINT('Ctrl Pts',(-6.6198706660591,7.1157124131703,-1.));
#6825=CARTESIAN_POINT('Ctrl Pts',(-6.60587239994885,7.05836882883084,-1.));
#6826=CARTESIAN_POINT('Ctrl Pts',(-6.5912030640433,7.00141528186886,-1.));
#6827=CARTESIAN_POINT('Ctrl Pts',(-6.5758359541656,6.94488033148854,-1.));
#6828=CARTESIAN_POINT('Ctrl Pts',(-6.55974857229919,6.88878938806037,-1.));
#6829=CARTESIAN_POINT('Ctrl Pts',(-6.54292981913304,6.83315901897031,-1.));
#6830=CARTESIAN_POINT('Ctrl Pts',(-6.52538888693355,6.77798990345397,-1.));
#6831=CARTESIAN_POINT('Ctrl Pts',(-6.50715912032692,6.72326378902152,-1.));
#6832=CARTESIAN_POINT('Ctrl Pts',(-6.48827758470622,6.66895976394944,-1.));
#6833=CARTESIAN_POINT('Ctrl Pts',(-6.46876645798849,6.6150690793574,-1.));
#6834=CARTESIAN_POINT('Ctrl Pts',(-6.44861636238489,6.56160843323028,-1.));
#6835=CARTESIAN_POINT('Ctrl Pts',(-6.42776254872513,6.50863892931077,-1.));
#6836=CARTESIAN_POINT('Ctrl Pts',(-6.40608444337878,6.45626649182453,-1.));
#6837=CARTESIAN_POINT('Ctrl Pts',(-6.38345478017075,6.404602962683,-1.));
#6838=CARTESIAN_POINT('Ctrl Pts',(-6.35978286360965,6.35373180396277,-1.));
#6839=CARTESIAN_POINT('Ctrl Pts',(-6.33505137069502,6.30367904881887,-1.));
#6840=CARTESIAN_POINT('Ctrl Pts',(-6.30937750420801,6.2543646376197,-1.));
#6841=CARTESIAN_POINT('Ctrl Pts',(-6.28297985424307,6.20562962932065,-1.));
#6842=CARTESIAN_POINT('Ctrl Pts',(-6.25605474467853,6.15733614814836,-1.));
#6843=CARTESIAN_POINT('Ctrl Pts',(-6.22866991793491,6.10945353793714,-1.));
#6844=CARTESIAN_POINT('Ctrl Pts',(-6.20066685685755,6.06213722636286,-1.));
#6845=CARTESIAN_POINT('Ctrl Pts',(-6.17151878498999,6.01584411654484,-1.));
#6846=CARTESIAN_POINT('Ctrl Pts',(-6.14045331140033,5.97123031969247,-1.));
#6847=CARTESIAN_POINT('Ctrl Pts',(-6.11342775487885,5.9374218385168,-1.));
#6848=CARTESIAN_POINT('Ctrl Pts',(-6.09164867072823,5.91336588048663,-1.));
#6849=CARTESIAN_POINT('Ctrl Pts',(-6.07642118935899,5.89793753402585,-1.));
#6850=CARTESIAN_POINT('Ctrl Pts',(-6.06863042059311,5.89037560471066,-1.));
#6851=CARTESIAN_POINT('',(-6.60014603862874,10.0218796774245,6.));
#6852=CARTESIAN_POINT('Ctrl Pts',(-6.60014603862877,10.0218796774244,6.));
#6853=CARTESIAN_POINT('Ctrl Pts',(-6.60293150665659,10.0085665785717,6.));
#6854=CARTESIAN_POINT('Ctrl Pts',(-6.60844558393656,9.98194823089968,6.));
#6855=CARTESIAN_POINT('Ctrl Pts',(-6.61654612354183,9.94204425953052,6.));
#6856=CARTESIAN_POINT('Ctrl Pts',(-6.62700557693596,9.88888607996273,6.));
#6857=CARTESIAN_POINT('Ctrl Pts',(-6.63951038900666,9.82251725114898,6.));
#6858=CARTESIAN_POINT('Ctrl Pts',(-6.65144464725859,9.75622826411013,6.));
#6859=CARTESIAN_POINT('Ctrl Pts',(-6.66280711160719,9.69002090483258,6.));
#6860=CARTESIAN_POINT('Ctrl Pts',(-6.67359647366961,9.62389802250188,6.));
#6861=CARTESIAN_POINT('Ctrl Pts',(-6.68381150859182,9.55786385494286,6.));
#6862=CARTESIAN_POINT('Ctrl Pts',(-6.69345108162377,9.49192378686253,6.));
#6863=CARTESIAN_POINT('Ctrl Pts',(-6.70251410760819,9.42608392519667,6.));
#6864=CARTESIAN_POINT('Ctrl Pts',(-6.71099953007123,9.36035072031876,6.));
#6865=CARTESIAN_POINT('Ctrl Pts',(-6.71890629646186,9.2947306015555,6.));
#6866=CARTESIAN_POINT('Ctrl Pts',(-6.72623333926845,9.22922952332026,6.));
#6867=CARTESIAN_POINT('Ctrl Pts',(-6.73297955932547,9.16385288053588,6.));
#6868=CARTESIAN_POINT('Ctrl Pts',(-6.73914381348523,9.09860577342166,6.));
#6869=CARTESIAN_POINT('Ctrl Pts',(-6.74472490424422,9.03349318036199,6.));
#6870=CARTESIAN_POINT('Ctrl Pts',(-6.74972157399229,8.96852015431046,6.));
#6871=CARTESIAN_POINT('Ctrl Pts',(-6.75413249860576,8.90369203916218,6.));
#6872=CARTESIAN_POINT('Ctrl Pts',(-6.75795629519249,8.83901457377471,6.));
#6873=CARTESIAN_POINT('Ctrl Pts',(-6.76119155448275,8.77449374557664,6.));
#6874=CARTESIAN_POINT('Ctrl Pts',(-6.76383687353852,8.71013569385599,6.));
#6875=CARTESIAN_POINT('Ctrl Pts',(-6.76589088878265,8.64594659806298,6.));
#6876=CARTESIAN_POINT('Ctrl Pts',(-6.76735232235634,8.5819325577994,6.));
#6877=CARTESIAN_POINT('Ctrl Pts',(-6.76822000004555,8.51809951610774,6.));
#6878=CARTESIAN_POINT('Ctrl Pts',(-6.76849272647565,8.45445340444926,6.));
#6879=CARTESIAN_POINT('Ctrl Pts',(-6.76816918165128,8.39100025749018,6.));
#6880=CARTESIAN_POINT('Ctrl Pts',(-6.76724781676282,8.32774633509908,6.));
#6881=CARTESIAN_POINT('Ctrl Pts',(-6.76572674650935,8.26469824786603,6.));
#6882=CARTESIAN_POINT('Ctrl Pts',(-6.7636036696164,8.20186305794855,6.));
#6883=CARTESIAN_POINT('Ctrl Pts',(-6.76087611417306,8.13924806419107,6.));
#6884=CARTESIAN_POINT('Ctrl Pts',(-6.75754166486089,8.07686060726828,6.));
#6885=CARTESIAN_POINT('Ctrl Pts',(-6.75359819949754,8.01470786732019,6.));
#6886=CARTESIAN_POINT('Ctrl Pts',(-6.7490441308376,7.95279665937614,6.));
#6887=CARTESIAN_POINT('Ctrl Pts',(-6.74387863902608,7.89113323756913,6.));
#6888=CARTESIAN_POINT('Ctrl Pts',(-6.73810106562748,7.82972378407324,6.));
#6889=CARTESIAN_POINT('Ctrl Pts',(-6.73171032576035,7.76857488460784,6.));
#6890=CARTESIAN_POINT('Ctrl Pts',(-6.72470431659336,7.70769400824503,6.));
#6891=CARTESIAN_POINT('Ctrl Pts',(-6.71707933277187,7.6470899828899,6.));
#6892=CARTESIAN_POINT('Ctrl Pts',(-6.70882947565318,7.58677347699226,6.));
#6893=CARTESIAN_POINT('Ctrl Pts',(-6.69994799095524,7.52675593674632,6.));
#6894=CARTESIAN_POINT('Ctrl Pts',(-6.69042862091104,7.46704851290034,6.));
#6895=CARTESIAN_POINT('Ctrl Pts',(-6.68026694677668,7.40766099640558,6.));
#6896=CARTESIAN_POINT('Ctrl Pts',(-6.66946176275797,7.34860073021492,6.));
#6897=CARTESIAN_POINT('Ctrl Pts',(-6.65801638970246,7.28987157005224,6.));
#6898=CARTESIAN_POINT('Ctrl Pts',(-6.64593535561053,7.23147652896403,6.));
#6899=CARTESIAN_POINT('Ctrl Pts',(-6.63322107969569,7.17342042004756,6.));
#6900=CARTESIAN_POINT('Ctrl Pts',(-6.6198706660591,7.1157124131703,6.));
#6901=CARTESIAN_POINT('Ctrl Pts',(-6.60587239994885,7.05836882883084,6.));
#6902=CARTESIAN_POINT('Ctrl Pts',(-6.5912030640433,7.00141528186886,6.));
#6903=CARTESIAN_POINT('Ctrl Pts',(-6.5758359541656,6.94488033148854,6.));
#6904=CARTESIAN_POINT('Ctrl Pts',(-6.55974857229919,6.88878938806037,6.));
#6905=CARTESIAN_POINT('Ctrl Pts',(-6.54292981913304,6.83315901897031,6.));
#6906=CARTESIAN_POINT('Ctrl Pts',(-6.52538888693355,6.77798990345397,6.));
#6907=CARTESIAN_POINT('Ctrl Pts',(-6.50715912032692,6.72326378902152,6.));
#6908=CARTESIAN_POINT('Ctrl Pts',(-6.48827758470622,6.66895976394944,6.));
#6909=CARTESIAN_POINT('Ctrl Pts',(-6.46876645798849,6.6150690793574,6.));
#6910=CARTESIAN_POINT('Ctrl Pts',(-6.44861636238489,6.56160843323028,6.));
#6911=CARTESIAN_POINT('Ctrl Pts',(-6.42776254872513,6.50863892931077,6.));
#6912=CARTESIAN_POINT('Ctrl Pts',(-6.40608444337878,6.45626649182453,6.));
#6913=CARTESIAN_POINT('Ctrl Pts',(-6.38345478017075,6.404602962683,6.));
#6914=CARTESIAN_POINT('Ctrl Pts',(-6.35978286360965,6.35373180396277,6.));
#6915=CARTESIAN_POINT('Ctrl Pts',(-6.33505137069502,6.30367904881887,6.));
#6916=CARTESIAN_POINT('Ctrl Pts',(-6.30937750420801,6.2543646376197,6.));
#6917=CARTESIAN_POINT('Ctrl Pts',(-6.28297985424307,6.20562962932065,6.));
#6918=CARTESIAN_POINT('Ctrl Pts',(-6.25605474467853,6.15733614814836,6.));
#6919=CARTESIAN_POINT('Ctrl Pts',(-6.22866991793491,6.10945353793714,6.));
#6920=CARTESIAN_POINT('Ctrl Pts',(-6.20066685685755,6.06213722636286,6.));
#6921=CARTESIAN_POINT('Ctrl Pts',(-6.17151878498999,6.01584411654484,6.));
#6922=CARTESIAN_POINT('Ctrl Pts',(-6.14045331140033,5.97123031969247,6.));
#6923=CARTESIAN_POINT('Ctrl Pts',(-6.11342775487885,5.9374218385168,6.));
#6924=CARTESIAN_POINT('Ctrl Pts',(-6.09164867072823,5.91336588048663,6.));
#6925=CARTESIAN_POINT('Ctrl Pts',(-6.07642118935899,5.89793753402585,6.));
#6926=CARTESIAN_POINT('Ctrl Pts',(-6.06863042059311,5.89037560471066,6.));
#6927=CARTESIAN_POINT('',(-6.60014603862874,10.0218796774245,0.));
#6928=CARTESIAN_POINT('Origin',(-1.99840144432528E-13,3.46133283549042E-13,
0.));
#6929=CARTESIAN_POINT('',(-5.37912937500617,10.726833976852,-1.));
#6930=CARTESIAN_POINT('Origin',(-1.99840144432528E-13,3.46133283549042E-13,
-1.));
#6931=CARTESIAN_POINT('',(-5.37912937500617,10.726833976852,6.));
#6932=CARTESIAN_POINT('Origin',(-1.99840144432528E-13,3.46133283549042E-13,
6.));
#6933=CARTESIAN_POINT('',(-5.37912937500617,10.726833976852,0.));
#6934=CARTESIAN_POINT('Ctrl Pts',(-2.066899701215,8.20077591276801,-3.75));
#6935=CARTESIAN_POINT('Ctrl Pts',(-2.066899701215,8.20077591276801,12.75));
#6936=CARTESIAN_POINT('Ctrl Pts',(-2.06955313972063,8.21130388109186,-3.75));
#6937=CARTESIAN_POINT('Ctrl Pts',(-2.06955313972063,8.21130388109186,12.75));
#6938=CARTESIAN_POINT('Ctrl Pts',(-2.07530073900944,8.23220544002367,-3.75));
#6939=CARTESIAN_POINT('Ctrl Pts',(-2.07530073900944,8.23220544002367,12.75));
#6940=CARTESIAN_POINT('Ctrl Pts',(-2.08524426770062,8.26309465918435,-3.75));
#6941=CARTESIAN_POINT('Ctrl Pts',(-2.08524426770062,8.26309465918435,12.75));
#6942=CARTESIAN_POINT('Ctrl Pts',(-2.10101049300138,8.3034037182712,-3.75));
#6943=CARTESIAN_POINT('Ctrl Pts',(-2.10101049300138,8.3034037182712,12.75));
#6944=CARTESIAN_POINT('Ctrl Pts',(-2.12411443763999,8.35261410600662,-3.75));
#6945=CARTESIAN_POINT('Ctrl Pts',(-2.12411443763999,8.35261410600662,12.75));
#6946=CARTESIAN_POINT('Ctrl Pts',(-2.1496314108288,8.40100363162428,-3.75));
#6947=CARTESIAN_POINT('Ctrl Pts',(-2.1496314108288,8.40100363162428,12.75));
#6948=CARTESIAN_POINT('Ctrl Pts',(-2.17660700812681,8.44891314968814,-3.75));
#6949=CARTESIAN_POINT('Ctrl Pts',(-2.17660700812681,8.44891314968814,12.75));
#6950=CARTESIAN_POINT('Ctrl Pts',(-2.20438215159743,8.49657041043196,-3.75));
#6951=CARTESIAN_POINT('Ctrl Pts',(-2.20438215159743,8.49657041043196,12.75));
#6952=CARTESIAN_POINT('Ctrl Pts',(-2.23274297834755,8.54403497990068,-3.75));
#6953=CARTESIAN_POINT('Ctrl Pts',(-2.23274297834755,8.54403497990068,12.75));
#6954=CARTESIAN_POINT('Ctrl Pts',(-2.26174990860571,8.59126351952004,-3.75));
#6955=CARTESIAN_POINT('Ctrl Pts',(-2.26174990860571,8.59126351952004,12.75));
#6956=CARTESIAN_POINT('Ctrl Pts',(-2.29162050823335,8.63815494571075,-3.75));
#6957=CARTESIAN_POINT('Ctrl Pts',(-2.29162050823335,8.63815494571075,12.75));
#6958=CARTESIAN_POINT('Ctrl Pts',(-2.32260171926006,8.68459942442029,-3.75));
#6959=CARTESIAN_POINT('Ctrl Pts',(-2.32260171926006,8.68459942442029,12.75));
#6960=CARTESIAN_POINT('Ctrl Pts',(-2.35482147675117,8.73053548487858,-3.75));
#6961=CARTESIAN_POINT('Ctrl Pts',(-2.35482147675117,8.73053548487858,12.75));
#6962=CARTESIAN_POINT('Ctrl Pts',(-2.38824857383288,8.77596511266658,-3.75));
#6963=CARTESIAN_POINT('Ctrl Pts',(-2.38824857383288,8.77596511266658,12.75));
#6964=CARTESIAN_POINT('Ctrl Pts',(-2.4227653824809,8.82092512134556,-3.75));
#6965=CARTESIAN_POINT('Ctrl Pts',(-2.4227653824809,8.82092512134556,12.75));
#6966=CARTESIAN_POINT('Ctrl Pts',(-2.45821141167118,8.86546980570045,-3.75));
#6967=CARTESIAN_POINT('Ctrl Pts',(-2.45821141167118,8.86546980570045,12.75));
#6968=CARTESIAN_POINT('Ctrl Pts',(-2.4944346415182,8.90965062344541,-3.75));
#6969=CARTESIAN_POINT('Ctrl Pts',(-2.4944346415182,8.90965062344541,12.75));
#6970=CARTESIAN_POINT('Ctrl Pts',(-2.53134978004337,8.95349309713545,-3.75));
#6971=CARTESIAN_POINT('Ctrl Pts',(-2.53134978004337,8.95349309713545,12.75));
#6972=CARTESIAN_POINT('Ctrl Pts',(-2.56893767747319,8.99699699918147,-3.75));
#6973=CARTESIAN_POINT('Ctrl Pts',(-2.56893767747319,8.99699699918147,12.75));
#6974=CARTESIAN_POINT('Ctrl Pts',(-2.60721699951879,9.0401474973841,-3.75));
#6975=CARTESIAN_POINT('Ctrl Pts',(-2.60721699951879,9.0401474973841,12.75));
#6976=CARTESIAN_POINT('Ctrl Pts',(-2.64622438896052,9.08292294803309,-3.75));
#6977=CARTESIAN_POINT('Ctrl Pts',(-2.64622438896052,9.08292294803309,12.75));
#6978=CARTESIAN_POINT('Ctrl Pts',(-2.68599232523134,9.12530360007999,-3.75));
#6979=CARTESIAN_POINT('Ctrl Pts',(-2.68599232523134,9.12530360007999,12.75));
#6980=CARTESIAN_POINT('Ctrl Pts',(-2.72652481622916,9.16728115317076,-3.75));
#6981=CARTESIAN_POINT('Ctrl Pts',(-2.72652481622916,9.16728115317076,12.75));
#6982=CARTESIAN_POINT('Ctrl Pts',(-2.76780196452137,9.20885693589776,-3.75));
#6983=CARTESIAN_POINT('Ctrl Pts',(-2.76780196452137,9.20885693589776,12.75));
#6984=CARTESIAN_POINT('Ctrl Pts',(-2.80979051507329,9.2500377269296,-3.75));
#6985=CARTESIAN_POINT('Ctrl Pts',(-2.80979051507329,9.2500377269296,12.75));
#6986=CARTESIAN_POINT('Ctrl Pts',(-2.85245238280019,9.29083237315974,-3.75));
#6987=CARTESIAN_POINT('Ctrl Pts',(-2.85245238280019,9.29083237315974,12.75));
#6988=CARTESIAN_POINT('Ctrl Pts',(-2.89575377593937,9.33124817395869,-3.75));
#6989=CARTESIAN_POINT('Ctrl Pts',(-2.89575377593937,9.33124817395869,12.75));
#6990=CARTESIAN_POINT('Ctrl Pts',(-2.9396747031485,9.3712871143499,-3.75));
#6991=CARTESIAN_POINT('Ctrl Pts',(-2.9396747031485,9.3712871143499,12.75));
#6992=CARTESIAN_POINT('Ctrl Pts',(-2.98420577513995,9.4109471173216,-3.75));
#6993=CARTESIAN_POINT('Ctrl Pts',(-2.98420577513995,9.4109471173216,12.75));
#6994=CARTESIAN_POINT('Ctrl Pts',(-3.029344033256,9.4502236812248,-3.75));
#6995=CARTESIAN_POINT('Ctrl Pts',(-3.029344033256,9.4502236812248,12.75));
#6996=CARTESIAN_POINT('Ctrl Pts',(-3.07508913212203,9.4891113781729,-3.75));
#6997=CARTESIAN_POINT('Ctrl Pts',(-3.07508913212203,9.4891113781729,12.75));
#6998=CARTESIAN_POINT('Ctrl Pts',(-3.12143939300699,9.52760540436562,-3.75));
#6999=CARTESIAN_POINT('Ctrl Pts',(-3.12143939300699,9.52760540436562,12.75));
#7000=CARTESIAN_POINT('Ctrl Pts',(-3.16838785383003,9.56570313257491,-3.75));
#7001=CARTESIAN_POINT('Ctrl Pts',(-3.16838785383003,9.56570313257491,12.75));
#7002=CARTESIAN_POINT('Ctrl Pts',(-3.2159238260067,9.60340349406962,-3.75));
#7003=CARTESIAN_POINT('Ctrl Pts',(-3.2159238260067,9.60340349406962,12.75));
#7004=CARTESIAN_POINT('Ctrl Pts',(-3.26403452382222,9.64070633286081,-3.75));
#7005=CARTESIAN_POINT('Ctrl Pts',(-3.26403452382222,9.64070633286081,12.75));
#7006=CARTESIAN_POINT('Ctrl Pts',(-3.31270665744062,9.67761177523124,-3.75));
#7007=CARTESIAN_POINT('Ctrl Pts',(-3.31270665744062,9.67761177523124,12.75));
#7008=CARTESIAN_POINT('Ctrl Pts',(-3.36192803839197,9.71411959533041,-3.75));
#7009=CARTESIAN_POINT('Ctrl Pts',(-3.36192803839197,9.71411959533041,12.75));
#7010=CARTESIAN_POINT('Ctrl Pts',(-3.41168916880891,9.75022858813702,-3.75));
#7011=CARTESIAN_POINT('Ctrl Pts',(-3.41168916880891,9.75022858813702,12.75));
#7012=CARTESIAN_POINT('Ctrl Pts',(-3.46198252886956,9.78593684022037,-3.75));
#7013=CARTESIAN_POINT('Ctrl Pts',(-3.46198252886956,9.78593684022037,12.75));
#7014=CARTESIAN_POINT('Ctrl Pts',(-3.51280187273295,9.8212419982557,-3.75));
#7015=CARTESIAN_POINT('Ctrl Pts',(-3.51280187273295,9.8212419982557,12.75));
#7016=CARTESIAN_POINT('Ctrl Pts',(-3.56414151726151,9.85614154137781,-3.75));
#7017=CARTESIAN_POINT('Ctrl Pts',(-3.56414151726151,9.85614154137781,12.75));
#7018=CARTESIAN_POINT('Ctrl Pts',(-3.61599563628969,9.89063305253546,-3.75));
#7019=CARTESIAN_POINT('Ctrl Pts',(-3.61599563628969,9.89063305253546,12.75));
#7020=CARTESIAN_POINT('Ctrl Pts',(-3.66835753420625,9.92471449880883,-3.75));
#7021=CARTESIAN_POINT('Ctrl Pts',(-3.66835753420625,9.92471449880883,12.75));
#7022=CARTESIAN_POINT('Ctrl Pts',(-3.72121993173636,9.95838412799173,-3.75));
#7023=CARTESIAN_POINT('Ctrl Pts',(-3.72121993173636,9.95838412799173,12.75));
#7024=CARTESIAN_POINT('Ctrl Pts',(-3.77457526401004,9.99164036147395,-3.75));
#7025=CARTESIAN_POINT('Ctrl Pts',(-3.77457526401004,9.99164036147395,12.75));
#7026=CARTESIAN_POINT('Ctrl Pts',(-3.82841597408715,10.0244816905709,-3.75));
#7027=CARTESIAN_POINT('Ctrl Pts',(-3.82841597408715,10.0244816905709,12.75));
#7028=CARTESIAN_POINT('Ctrl Pts',(-3.88273479532262,10.056906577166,-3.75));
#7029=CARTESIAN_POINT('Ctrl Pts',(-3.88273479532262,10.056906577166,12.75));
#7030=CARTESIAN_POINT('Ctrl Pts',(-3.93752506012706,10.0889133486827,-3.75));
#7031=CARTESIAN_POINT('Ctrl Pts',(-3.93752506012706,10.0889133486827,12.75));
#7032=CARTESIAN_POINT('Ctrl Pts',(-3.99278057289046,10.1205002164952,-3.75));
#7033=CARTESIAN_POINT('Ctrl Pts',(-3.99278057289046,10.1205002164952,12.75));
#7034=CARTESIAN_POINT('Ctrl Pts',(-4.04849544744087,10.1516653064199,-3.75));
#7035=CARTESIAN_POINT('Ctrl Pts',(-4.04849544744087,10.1516653064199,12.75));
#7036=CARTESIAN_POINT('Ctrl Pts',(-4.10466394929486,10.1824066879509,-3.75));
#7037=CARTESIAN_POINT('Ctrl Pts',(-4.10466394929486,10.1824066879509,12.75));
#7038=CARTESIAN_POINT('Ctrl Pts',(-4.16128034451962,10.2127224064663,-3.75));
#7039=CARTESIAN_POINT('Ctrl Pts',(-4.16128034451962,10.2127224064663,12.75));
#7040=CARTESIAN_POINT('Ctrl Pts',(-4.21833871177567,10.2426105188232,-3.75));
#7041=CARTESIAN_POINT('Ctrl Pts',(-4.21833871177567,10.2426105188232,12.75));
#7042=CARTESIAN_POINT('Ctrl Pts',(-4.27583301771353,10.272069116189,-3.75));
#7043=CARTESIAN_POINT('Ctrl Pts',(-4.27583301771353,10.272069116189,12.75));
#7044=CARTESIAN_POINT('Ctrl Pts',(-4.33375724408483,10.3010963438997,-3.75));
#7045=CARTESIAN_POINT('Ctrl Pts',(-4.33375724408483,10.3010963438997,12.75));
#7046=CARTESIAN_POINT('Ctrl Pts',(-4.39210550098945,10.3296904287044,-3.75));
#7047=CARTESIAN_POINT('Ctrl Pts',(-4.39210550098945,10.3296904287044,12.75));
#7048=CARTESIAN_POINT('Ctrl Pts',(-4.45087212698485,10.3578496987941,-3.75));
#7049=CARTESIAN_POINT('Ctrl Pts',(-4.45087212698485,10.3578496987941,12.75));
#7050=CARTESIAN_POINT('Ctrl Pts',(-4.5100518320603,10.3855726289458,-3.75));
#7051=CARTESIAN_POINT('Ctrl Pts',(-4.5100518320603,10.3855726289458,12.75));
#7052=CARTESIAN_POINT('Ctrl Pts',(-4.56963961142454,10.4128577818052,-3.75));
#7053=CARTESIAN_POINT('Ctrl Pts',(-4.56963961142454,10.4128577818052,12.75));
#7054=CARTESIAN_POINT('Ctrl Pts',(-4.62963055491846,10.4397037052484,-3.75));
#7055=CARTESIAN_POINT('Ctrl Pts',(-4.62963055491846,10.4397037052484,12.75));
#7056=CARTESIAN_POINT('Ctrl Pts',(-4.69001967404875,10.4661088391609,-3.75));
#7057=CARTESIAN_POINT('Ctrl Pts',(-4.69001967404875,10.4661088391609,12.75));
#7058=CARTESIAN_POINT('Ctrl Pts',(-4.7508017470924,10.4920714379865,-3.75));
#7059=CARTESIAN_POINT('Ctrl Pts',(-4.7508017470924,10.4920714379865,12.75));
#7060=CARTESIAN_POINT('Ctrl Pts',(-4.81197108362035,10.5175894490106,-3.75));
#7061=CARTESIAN_POINT('Ctrl Pts',(-4.81197108362035,10.5175894490106,12.75));
#7062=CARTESIAN_POINT('Ctrl Pts',(-4.87352158939686,10.5426605691059,-3.75));
#7063=CARTESIAN_POINT('Ctrl Pts',(-4.87352158939686,10.5426605691059,12.75));
#7064=CARTESIAN_POINT('Ctrl Pts',(-4.93544714999767,10.5672824880187,-3.75));
#7065=CARTESIAN_POINT('Ctrl Pts',(-4.93544714999767,10.5672824880187,12.75));
#7066=CARTESIAN_POINT('Ctrl Pts',(-4.99774193408264,10.5914530920551,-3.75));
#7067=CARTESIAN_POINT('Ctrl Pts',(-4.99774193408264,10.5914530920551,12.75));
#7068=CARTESIAN_POINT('Ctrl Pts',(-5.06040071098369,10.6151706715837,-3.75));
#7069=CARTESIAN_POINT('Ctrl Pts',(-5.06040071098369,10.6151706715837,12.75));
#7070=CARTESIAN_POINT('Ctrl Pts',(-5.12341919820983,10.638434168447,-3.75));
#7071=CARTESIAN_POINT('Ctrl Pts',(-5.12341919820983,10.638434168447,12.75));
#7072=CARTESIAN_POINT('Ctrl Pts',(-5.18679427410258,10.661243291145,-3.75));
#7073=CARTESIAN_POINT('Ctrl Pts',(-5.18679427410258,10.661243291145,12.75));
#7074=CARTESIAN_POINT('Ctrl Pts',(-5.25052377191006,10.6835982206291,-3.75));
#7075=CARTESIAN_POINT('Ctrl Pts',(-5.25052377191006,10.6835982206291,12.75));
#7076=CARTESIAN_POINT('Ctrl Pts',(-5.30178983253176,10.7011191580639,-3.75));
#7077=CARTESIAN_POINT('Ctrl Pts',(-5.30178983253176,10.7011191580639,12.75));
#7078=CARTESIAN_POINT('Ctrl Pts',(-5.34039795525198,10.714055870666,-3.75));
#7079=CARTESIAN_POINT('Ctrl Pts',(-5.34039795525198,10.714055870666,12.75));
#7080=CARTESIAN_POINT('Ctrl Pts',(-5.3662071591827,10.7225897134991,-3.75));
#7081=CARTESIAN_POINT('Ctrl Pts',(-5.3662071591827,10.7225897134991,12.75));
#7082=CARTESIAN_POINT('Ctrl Pts',(-5.37912937500617,10.726833976852,-3.75));
#7083=CARTESIAN_POINT('Ctrl Pts',(-5.37912937500617,10.726833976852,12.75));
#7084=CARTESIAN_POINT('Ctrl Pts',(-2.066899701215,8.20077591276801,-1.));
#7085=CARTESIAN_POINT('Ctrl Pts',(-2.06955313972063,8.21130388109186,-1.));
#7086=CARTESIAN_POINT('Ctrl Pts',(-2.07530073900944,8.23220544002367,-1.));
#7087=CARTESIAN_POINT('Ctrl Pts',(-2.08524426770062,8.26309465918435,-1.));
#7088=CARTESIAN_POINT('Ctrl Pts',(-2.10101049300138,8.3034037182712,-1.));
#7089=CARTESIAN_POINT('Ctrl Pts',(-2.12411443763999,8.35261410600662,-1.));
#7090=CARTESIAN_POINT('Ctrl Pts',(-2.1496314108288,8.40100363162428,-1.));
#7091=CARTESIAN_POINT('Ctrl Pts',(-2.17660700812681,8.44891314968814,-1.));
#7092=CARTESIAN_POINT('Ctrl Pts',(-2.20438215159743,8.49657041043196,-1.));
#7093=CARTESIAN_POINT('Ctrl Pts',(-2.23274297834755,8.54403497990068,-1.));
#7094=CARTESIAN_POINT('Ctrl Pts',(-2.26174990860571,8.59126351952004,-1.));
#7095=CARTESIAN_POINT('Ctrl Pts',(-2.29162050823335,8.63815494571075,-1.));
#7096=CARTESIAN_POINT('Ctrl Pts',(-2.32260171926006,8.68459942442029,-1.));
#7097=CARTESIAN_POINT('Ctrl Pts',(-2.35482147675117,8.73053548487858,-1.));
#7098=CARTESIAN_POINT('Ctrl Pts',(-2.38824857383288,8.77596511266658,-1.));
#7099=CARTESIAN_POINT('Ctrl Pts',(-2.4227653824809,8.82092512134556,-1.));
#7100=CARTESIAN_POINT('Ctrl Pts',(-2.45821141167118,8.86546980570045,-1.));
#7101=CARTESIAN_POINT('Ctrl Pts',(-2.4944346415182,8.90965062344541,-1.));
#7102=CARTESIAN_POINT('Ctrl Pts',(-2.53134978004337,8.95349309713545,-1.));
#7103=CARTESIAN_POINT('Ctrl Pts',(-2.56893767747319,8.99699699918147,-1.));
#7104=CARTESIAN_POINT('Ctrl Pts',(-2.60721699951879,9.0401474973841,-1.));
#7105=CARTESIAN_POINT('Ctrl Pts',(-2.64622438896052,9.08292294803309,-1.));
#7106=CARTESIAN_POINT('Ctrl Pts',(-2.68599232523134,9.12530360007999,-1.));
#7107=CARTESIAN_POINT('Ctrl Pts',(-2.72652481622916,9.16728115317076,-1.));
#7108=CARTESIAN_POINT('Ctrl Pts',(-2.76780196452137,9.20885693589776,-1.));
#7109=CARTESIAN_POINT('Ctrl Pts',(-2.80979051507329,9.2500377269296,-1.));
#7110=CARTESIAN_POINT('Ctrl Pts',(-2.85245238280019,9.29083237315974,-1.));
#7111=CARTESIAN_POINT('Ctrl Pts',(-2.89575377593937,9.33124817395869,-1.));
#7112=CARTESIAN_POINT('Ctrl Pts',(-2.9396747031485,9.3712871143499,-1.));
#7113=CARTESIAN_POINT('Ctrl Pts',(-2.98420577513995,9.4109471173216,-1.));
#7114=CARTESIAN_POINT('Ctrl Pts',(-3.029344033256,9.4502236812248,-1.));
#7115=CARTESIAN_POINT('Ctrl Pts',(-3.07508913212203,9.4891113781729,-1.));
#7116=CARTESIAN_POINT('Ctrl Pts',(-3.12143939300699,9.52760540436562,-1.));
#7117=CARTESIAN_POINT('Ctrl Pts',(-3.16838785383003,9.56570313257491,-1.));
#7118=CARTESIAN_POINT('Ctrl Pts',(-3.2159238260067,9.60340349406962,-1.));
#7119=CARTESIAN_POINT('Ctrl Pts',(-3.26403452382222,9.64070633286081,-1.));
#7120=CARTESIAN_POINT('Ctrl Pts',(-3.31270665744062,9.67761177523124,-1.));
#7121=CARTESIAN_POINT('Ctrl Pts',(-3.36192803839197,9.71411959533041,-1.));
#7122=CARTESIAN_POINT('Ctrl Pts',(-3.41168916880891,9.75022858813702,-1.));
#7123=CARTESIAN_POINT('Ctrl Pts',(-3.46198252886956,9.78593684022037,-1.));
#7124=CARTESIAN_POINT('Ctrl Pts',(-3.51280187273295,9.8212419982557,-1.));
#7125=CARTESIAN_POINT('Ctrl Pts',(-3.56414151726151,9.85614154137781,-1.));
#7126=CARTESIAN_POINT('Ctrl Pts',(-3.61599563628969,9.89063305253546,-1.));
#7127=CARTESIAN_POINT('Ctrl Pts',(-3.66835753420625,9.92471449880883,-1.));
#7128=CARTESIAN_POINT('Ctrl Pts',(-3.72121993173636,9.95838412799173,-1.));
#7129=CARTESIAN_POINT('Ctrl Pts',(-3.77457526401004,9.99164036147395,-1.));
#7130=CARTESIAN_POINT('Ctrl Pts',(-3.82841597408715,10.0244816905709,-1.));
#7131=CARTESIAN_POINT('Ctrl Pts',(-3.88273479532262,10.056906577166,-1.));
#7132=CARTESIAN_POINT('Ctrl Pts',(-3.93752506012706,10.0889133486827,-1.));
#7133=CARTESIAN_POINT('Ctrl Pts',(-3.99278057289046,10.1205002164952,-1.));
#7134=CARTESIAN_POINT('Ctrl Pts',(-4.04849544744087,10.1516653064199,-1.));
#7135=CARTESIAN_POINT('Ctrl Pts',(-4.10466394929486,10.1824066879509,-1.));
#7136=CARTESIAN_POINT('Ctrl Pts',(-4.16128034451962,10.2127224064663,-1.));
#7137=CARTESIAN_POINT('Ctrl Pts',(-4.21833871177567,10.2426105188232,-1.));
#7138=CARTESIAN_POINT('Ctrl Pts',(-4.27583301771353,10.272069116189,-1.));
#7139=CARTESIAN_POINT('Ctrl Pts',(-4.33375724408483,10.3010963438997,-1.));
#7140=CARTESIAN_POINT('Ctrl Pts',(-4.39210550098945,10.3296904287044,-1.));
#7141=CARTESIAN_POINT('Ctrl Pts',(-4.45087212698485,10.3578496987941,-1.));
#7142=CARTESIAN_POINT('Ctrl Pts',(-4.5100518320603,10.3855726289458,-1.));
#7143=CARTESIAN_POINT('Ctrl Pts',(-4.56963961142454,10.4128577818052,-1.));
#7144=CARTESIAN_POINT('Ctrl Pts',(-4.62963055491846,10.4397037052484,-1.));
#7145=CARTESIAN_POINT('Ctrl Pts',(-4.69001967404875,10.4661088391609,-1.));
#7146=CARTESIAN_POINT('Ctrl Pts',(-4.7508017470924,10.4920714379865,-1.));
#7147=CARTESIAN_POINT('Ctrl Pts',(-4.81197108362035,10.5175894490106,-1.));
#7148=CARTESIAN_POINT('Ctrl Pts',(-4.87352158939686,10.5426605691059,-1.));
#7149=CARTESIAN_POINT('Ctrl Pts',(-4.93544714999767,10.5672824880187,-1.));
#7150=CARTESIAN_POINT('Ctrl Pts',(-4.99774193408264,10.5914530920551,-1.));
#7151=CARTESIAN_POINT('Ctrl Pts',(-5.06040071098369,10.6151706715837,-1.));
#7152=CARTESIAN_POINT('Ctrl Pts',(-5.12341919820983,10.638434168447,-1.));
#7153=CARTESIAN_POINT('Ctrl Pts',(-5.18679427410258,10.661243291145,-1.));
#7154=CARTESIAN_POINT('Ctrl Pts',(-5.25052377191006,10.6835982206291,-1.));
#7155=CARTESIAN_POINT('Ctrl Pts',(-5.30178983253176,10.7011191580639,-1.));
#7156=CARTESIAN_POINT('Ctrl Pts',(-5.34039795525198,10.714055870666,-1.));
#7157=CARTESIAN_POINT('Ctrl Pts',(-5.3662071591827,10.7225897134991,-1.));
#7158=CARTESIAN_POINT('Ctrl Pts',(-5.37912937500617,10.726833976852,-1.));
#7159=CARTESIAN_POINT('Ctrl Pts',(-2.066899701215,8.20077591276801,6.));
#7160=CARTESIAN_POINT('Ctrl Pts',(-2.06955313972063,8.21130388109186,6.));
#7161=CARTESIAN_POINT('Ctrl Pts',(-2.07530073900944,8.23220544002367,6.));
#7162=CARTESIAN_POINT('Ctrl Pts',(-2.08524426770062,8.26309465918435,6.));
#7163=CARTESIAN_POINT('Ctrl Pts',(-2.10101049300138,8.3034037182712,6.));
#7164=CARTESIAN_POINT('Ctrl Pts',(-2.12411443763999,8.35261410600662,6.));
#7165=CARTESIAN_POINT('Ctrl Pts',(-2.1496314108288,8.40100363162428,6.));
#7166=CARTESIAN_POINT('Ctrl Pts',(-2.17660700812681,8.44891314968814,6.));
#7167=CARTESIAN_POINT('Ctrl Pts',(-2.20438215159743,8.49657041043196,6.));
#7168=CARTESIAN_POINT('Ctrl Pts',(-2.23274297834755,8.54403497990068,6.));
#7169=CARTESIAN_POINT('Ctrl Pts',(-2.26174990860571,8.59126351952004,6.));
#7170=CARTESIAN_POINT('Ctrl Pts',(-2.29162050823335,8.63815494571075,6.));
#7171=CARTESIAN_POINT('Ctrl Pts',(-2.32260171926006,8.68459942442029,6.));
#7172=CARTESIAN_POINT('Ctrl Pts',(-2.35482147675117,8.73053548487858,6.));
#7173=CARTESIAN_POINT('Ctrl Pts',(-2.38824857383288,8.77596511266658,6.));
#7174=CARTESIAN_POINT('Ctrl Pts',(-2.4227653824809,8.82092512134556,6.));
#7175=CARTESIAN_POINT('Ctrl Pts',(-2.45821141167118,8.86546980570045,6.));
#7176=CARTESIAN_POINT('Ctrl Pts',(-2.4944346415182,8.90965062344541,6.));
#7177=CARTESIAN_POINT('Ctrl Pts',(-2.53134978004337,8.95349309713545,6.));
#7178=CARTESIAN_POINT('Ctrl Pts',(-2.56893767747319,8.99699699918147,6.));
#7179=CARTESIAN_POINT('Ctrl Pts',(-2.60721699951879,9.0401474973841,6.));
#7180=CARTESIAN_POINT('Ctrl Pts',(-2.64622438896052,9.08292294803309,6.));
#7181=CARTESIAN_POINT('Ctrl Pts',(-2.68599232523134,9.12530360007999,6.));
#7182=CARTESIAN_POINT('Ctrl Pts',(-2.72652481622916,9.16728115317076,6.));
#7183=CARTESIAN_POINT('Ctrl Pts',(-2.76780196452137,9.20885693589776,6.));
#7184=CARTESIAN_POINT('Ctrl Pts',(-2.80979051507329,9.2500377269296,6.));
#7185=CARTESIAN_POINT('Ctrl Pts',(-2.85245238280019,9.29083237315974,6.));
#7186=CARTESIAN_POINT('Ctrl Pts',(-2.89575377593937,9.33124817395869,6.));
#7187=CARTESIAN_POINT('Ctrl Pts',(-2.9396747031485,9.3712871143499,6.));
#7188=CARTESIAN_POINT('Ctrl Pts',(-2.98420577513995,9.4109471173216,6.));
#7189=CARTESIAN_POINT('Ctrl Pts',(-3.029344033256,9.4502236812248,6.));
#7190=CARTESIAN_POINT('Ctrl Pts',(-3.07508913212203,9.4891113781729,6.));
#7191=CARTESIAN_POINT('Ctrl Pts',(-3.12143939300699,9.52760540436562,6.));
#7192=CARTESIAN_POINT('Ctrl Pts',(-3.16838785383003,9.56570313257491,6.));
#7193=CARTESIAN_POINT('Ctrl Pts',(-3.2159238260067,9.60340349406962,6.));
#7194=CARTESIAN_POINT('Ctrl Pts',(-3.26403452382222,9.64070633286081,6.));
#7195=CARTESIAN_POINT('Ctrl Pts',(-3.31270665744062,9.67761177523124,6.));
#7196=CARTESIAN_POINT('Ctrl Pts',(-3.36192803839197,9.71411959533041,6.));
#7197=CARTESIAN_POINT('Ctrl Pts',(-3.41168916880891,9.75022858813702,6.));
#7198=CARTESIAN_POINT('Ctrl Pts',(-3.46198252886956,9.78593684022037,6.));
#7199=CARTESIAN_POINT('Ctrl Pts',(-3.51280187273295,9.8212419982557,6.));
#7200=CARTESIAN_POINT('Ctrl Pts',(-3.56414151726151,9.85614154137781,6.));
#7201=CARTESIAN_POINT('Ctrl Pts',(-3.61599563628969,9.89063305253546,6.));
#7202=CARTESIAN_POINT('Ctrl Pts',(-3.66835753420625,9.92471449880883,6.));
#7203=CARTESIAN_POINT('Ctrl Pts',(-3.72121993173636,9.95838412799173,6.));
#7204=CARTESIAN_POINT('Ctrl Pts',(-3.77457526401004,9.99164036147395,6.));
#7205=CARTESIAN_POINT('Ctrl Pts',(-3.82841597408715,10.0244816905709,6.));
#7206=CARTESIAN_POINT('Ctrl Pts',(-3.88273479532262,10.056906577166,6.));
#7207=CARTESIAN_POINT('Ctrl Pts',(-3.93752506012706,10.0889133486827,6.));
#7208=CARTESIAN_POINT('Ctrl Pts',(-3.99278057289046,10.1205002164952,6.));
#7209=CARTESIAN_POINT('Ctrl Pts',(-4.04849544744087,10.1516653064199,6.));
#7210=CARTESIAN_POINT('Ctrl Pts',(-4.10466394929486,10.1824066879509,6.));
#7211=CARTESIAN_POINT('Ctrl Pts',(-4.16128034451962,10.2127224064663,6.));
#7212=CARTESIAN_POINT('Ctrl Pts',(-4.21833871177567,10.2426105188232,6.));
#7213=CARTESIAN_POINT('Ctrl Pts',(-4.27583301771353,10.272069116189,6.));
#7214=CARTESIAN_POINT('Ctrl Pts',(-4.33375724408483,10.3010963438997,6.));
#7215=CARTESIAN_POINT('Ctrl Pts',(-4.39210550098945,10.3296904287044,6.));
#7216=CARTESIAN_POINT('Ctrl Pts',(-4.45087212698485,10.3578496987941,6.));
#7217=CARTESIAN_POINT('Ctrl Pts',(-4.5100518320603,10.3855726289458,6.));
#7218=CARTESIAN_POINT('Ctrl Pts',(-4.56963961142454,10.4128577818052,6.));
#7219=CARTESIAN_POINT('Ctrl Pts',(-4.62963055491846,10.4397037052484,6.));
#7220=CARTESIAN_POINT('Ctrl Pts',(-4.69001967404875,10.4661088391609,6.));
#7221=CARTESIAN_POINT('Ctrl Pts',(-4.7508017470924,10.4920714379865,6.));
#7222=CARTESIAN_POINT('Ctrl Pts',(-4.81197108362035,10.5175894490106,6.));
#7223=CARTESIAN_POINT('Ctrl Pts',(-4.87352158939686,10.5426605691059,6.));
#7224=CARTESIAN_POINT('Ctrl Pts',(-4.93544714999767,10.5672824880187,6.));
#7225=CARTESIAN_POINT('Ctrl Pts',(-4.99774193408264,10.5914530920551,6.));
#7226=CARTESIAN_POINT('Ctrl Pts',(-5.06040071098369,10.6151706715837,6.));
#7227=CARTESIAN_POINT('Ctrl Pts',(-5.12341919820983,10.638434168447,6.));
#7228=CARTESIAN_POINT('Ctrl Pts',(-5.18679427410258,10.661243291145,6.));
#7229=CARTESIAN_POINT('Ctrl Pts',(-5.25052377191006,10.6835982206291,6.));
#7230=CARTESIAN_POINT('Ctrl Pts',(-5.30178983253176,10.7011191580639,6.));
#7231=CARTESIAN_POINT('Ctrl Pts',(-5.34039795525198,10.714055870666,6.));
#7232=CARTESIAN_POINT('Ctrl Pts',(-5.3662071591827,10.7225897134991,6.));
#7233=CARTESIAN_POINT('Ctrl Pts',(-5.37912937500617,10.726833976852,6.));
#7234=CARTESIAN_POINT('Ctrl Pts',(5.37912937500617,10.726833976852,-3.75));
#7235=CARTESIAN_POINT('Ctrl Pts',(5.37912937500617,10.726833976852,12.75));
#7236=CARTESIAN_POINT('Ctrl Pts',(5.36620715918271,10.7225897134991,-3.75));
#7237=CARTESIAN_POINT('Ctrl Pts',(5.36620715918271,10.7225897134991,12.75));
#7238=CARTESIAN_POINT('Ctrl Pts',(5.34039795525198,10.714055870666,-3.75));
#7239=CARTESIAN_POINT('Ctrl Pts',(5.34039795525198,10.714055870666,12.75));
#7240=CARTESIAN_POINT('Ctrl Pts',(5.30178983253176,10.7011191580639,-3.75));
#7241=CARTESIAN_POINT('Ctrl Pts',(5.30178983253176,10.7011191580639,12.75));
#7242=CARTESIAN_POINT('Ctrl Pts',(5.25052377191006,10.6835982206291,-3.75));
#7243=CARTESIAN_POINT('Ctrl Pts',(5.25052377191006,10.6835982206291,12.75));
#7244=CARTESIAN_POINT('Ctrl Pts',(5.18679427410258,10.661243291145,-3.75));
#7245=CARTESIAN_POINT('Ctrl Pts',(5.18679427410258,10.661243291145,12.75));
#7246=CARTESIAN_POINT('Ctrl Pts',(5.12341919820984,10.638434168447,-3.75));
#7247=CARTESIAN_POINT('Ctrl Pts',(5.12341919820984,10.638434168447,12.75));
#7248=CARTESIAN_POINT('Ctrl Pts',(5.06040071098369,10.6151706715837,-3.75));
#7249=CARTESIAN_POINT('Ctrl Pts',(5.06040071098369,10.6151706715837,12.75));
#7250=CARTESIAN_POINT('Ctrl Pts',(4.99774193408264,10.5914530920551,-3.75));
#7251=CARTESIAN_POINT('Ctrl Pts',(4.99774193408264,10.5914530920551,12.75));
#7252=CARTESIAN_POINT('Ctrl Pts',(4.93544714999767,10.5672824880187,-3.75));
#7253=CARTESIAN_POINT('Ctrl Pts',(4.93544714999767,10.5672824880187,12.75));
#7254=CARTESIAN_POINT('Ctrl Pts',(4.87352158939686,10.5426605691059,-3.75));
#7255=CARTESIAN_POINT('Ctrl Pts',(4.87352158939686,10.5426605691059,12.75));
#7256=CARTESIAN_POINT('Ctrl Pts',(4.81197108362035,10.5175894490106,-3.75));
#7257=CARTESIAN_POINT('Ctrl Pts',(4.81197108362035,10.5175894490106,12.75));
#7258=CARTESIAN_POINT('Ctrl Pts',(4.7508017470924,10.4920714379865,-3.75));
#7259=CARTESIAN_POINT('Ctrl Pts',(4.7508017470924,10.4920714379865,12.75));
#7260=CARTESIAN_POINT('Ctrl Pts',(4.69001967404875,10.4661088391609,-3.75));
#7261=CARTESIAN_POINT('Ctrl Pts',(4.69001967404875,10.4661088391609,12.75));
#7262=CARTESIAN_POINT('Ctrl Pts',(4.62963055491846,10.4397037052484,-3.75));
#7263=CARTESIAN_POINT('Ctrl Pts',(4.62963055491846,10.4397037052484,12.75));
#7264=CARTESIAN_POINT('Ctrl Pts',(4.56963961142454,10.4128577818052,-3.75));
#7265=CARTESIAN_POINT('Ctrl Pts',(4.56963961142454,10.4128577818052,12.75));
#7266=CARTESIAN_POINT('Ctrl Pts',(4.5100518320603,10.3855726289458,-3.75));
#7267=CARTESIAN_POINT('Ctrl Pts',(4.5100518320603,10.3855726289458,12.75));
#7268=CARTESIAN_POINT('Ctrl Pts',(4.45087212698485,10.3578496987941,-3.75));
#7269=CARTESIAN_POINT('Ctrl Pts',(4.45087212698485,10.3578496987941,12.75));
#7270=CARTESIAN_POINT('Ctrl Pts',(4.39210550098945,10.3296904287044,-3.75));
#7271=CARTESIAN_POINT('Ctrl Pts',(4.39210550098945,10.3296904287044,12.75));
#7272=CARTESIAN_POINT('Ctrl Pts',(4.33375724408484,10.3010963438997,-3.75));
#7273=CARTESIAN_POINT('Ctrl Pts',(4.33375724408484,10.3010963438997,12.75));
#7274=CARTESIAN_POINT('Ctrl Pts',(4.27583301771353,10.272069116189,-3.75));
#7275=CARTESIAN_POINT('Ctrl Pts',(4.27583301771353,10.272069116189,12.75));
#7276=CARTESIAN_POINT('Ctrl Pts',(4.21833871177567,10.2426105188232,-3.75));
#7277=CARTESIAN_POINT('Ctrl Pts',(4.21833871177567,10.2426105188232,12.75));
#7278=CARTESIAN_POINT('Ctrl Pts',(4.16128034451962,10.2127224064663,-3.75));
#7279=CARTESIAN_POINT('Ctrl Pts',(4.16128034451962,10.2127224064663,12.75));
#7280=CARTESIAN_POINT('Ctrl Pts',(4.10466394929486,10.1824066879509,-3.75));
#7281=CARTESIAN_POINT('Ctrl Pts',(4.10466394929486,10.1824066879509,12.75));
#7282=CARTESIAN_POINT('Ctrl Pts',(4.04849544744087,10.1516653064199,-3.75));
#7283=CARTESIAN_POINT('Ctrl Pts',(4.04849544744087,10.1516653064199,12.75));
#7284=CARTESIAN_POINT('Ctrl Pts',(3.99278057289046,10.1205002164952,-3.75));
#7285=CARTESIAN_POINT('Ctrl Pts',(3.99278057289046,10.1205002164952,12.75));
#7286=CARTESIAN_POINT('Ctrl Pts',(3.93752506012707,10.0889133486827,-3.75));
#7287=CARTESIAN_POINT('Ctrl Pts',(3.93752506012707,10.0889133486827,12.75));
#7288=CARTESIAN_POINT('Ctrl Pts',(3.88273479532263,10.056906577166,-3.75));
#7289=CARTESIAN_POINT('Ctrl Pts',(3.88273479532263,10.056906577166,12.75));
#7290=CARTESIAN_POINT('Ctrl Pts',(3.82841597408715,10.0244816905709,-3.75));
#7291=CARTESIAN_POINT('Ctrl Pts',(3.82841597408715,10.0244816905709,12.75));
#7292=CARTESIAN_POINT('Ctrl Pts',(3.77457526401004,9.99164036147395,-3.75));
#7293=CARTESIAN_POINT('Ctrl Pts',(3.77457526401004,9.99164036147395,12.75));
#7294=CARTESIAN_POINT('Ctrl Pts',(3.72121993173636,9.95838412799172,-3.75));
#7295=CARTESIAN_POINT('Ctrl Pts',(3.72121993173636,9.95838412799172,12.75));
#7296=CARTESIAN_POINT('Ctrl Pts',(3.66835753420625,9.92471449880883,-3.75));
#7297=CARTESIAN_POINT('Ctrl Pts',(3.66835753420625,9.92471449880883,12.75));
#7298=CARTESIAN_POINT('Ctrl Pts',(3.61599563628969,9.89063305253546,-3.75));
#7299=CARTESIAN_POINT('Ctrl Pts',(3.61599563628969,9.89063305253546,12.75));
#7300=CARTESIAN_POINT('Ctrl Pts',(3.56414151726151,9.85614154137781,-3.75));
#7301=CARTESIAN_POINT('Ctrl Pts',(3.56414151726151,9.85614154137781,12.75));
#7302=CARTESIAN_POINT('Ctrl Pts',(3.51280187273295,9.8212419982557,-3.75));
#7303=CARTESIAN_POINT('Ctrl Pts',(3.51280187273295,9.8212419982557,12.75));
#7304=CARTESIAN_POINT('Ctrl Pts',(3.46198252886957,9.78593684022037,-3.75));
#7305=CARTESIAN_POINT('Ctrl Pts',(3.46198252886957,9.78593684022037,12.75));
#7306=CARTESIAN_POINT('Ctrl Pts',(3.41168916880891,9.75022858813702,-3.75));
#7307=CARTESIAN_POINT('Ctrl Pts',(3.41168916880891,9.75022858813702,12.75));
#7308=CARTESIAN_POINT('Ctrl Pts',(3.36192803839197,9.7141195953304,-3.75));
#7309=CARTESIAN_POINT('Ctrl Pts',(3.36192803839197,9.7141195953304,12.75));
#7310=CARTESIAN_POINT('Ctrl Pts',(3.31270665744062,9.67761177523123,-3.75));
#7311=CARTESIAN_POINT('Ctrl Pts',(3.31270665744062,9.67761177523123,12.75));
#7312=CARTESIAN_POINT('Ctrl Pts',(3.26403452382222,9.64070633286081,-3.75));
#7313=CARTESIAN_POINT('Ctrl Pts',(3.26403452382222,9.64070633286081,12.75));
#7314=CARTESIAN_POINT('Ctrl Pts',(3.2159238260067,9.60340349406962,-3.75));
#7315=CARTESIAN_POINT('Ctrl Pts',(3.2159238260067,9.60340349406962,12.75));
#7316=CARTESIAN_POINT('Ctrl Pts',(3.16838785383004,9.56570313257491,-3.75));
#7317=CARTESIAN_POINT('Ctrl Pts',(3.16838785383004,9.56570313257491,12.75));
#7318=CARTESIAN_POINT('Ctrl Pts',(3.12143939300699,9.52760540436562,-3.75));
#7319=CARTESIAN_POINT('Ctrl Pts',(3.12143939300699,9.52760540436562,12.75));
#7320=CARTESIAN_POINT('Ctrl Pts',(3.07508913212204,9.4891113781729,-3.75));
#7321=CARTESIAN_POINT('Ctrl Pts',(3.07508913212204,9.4891113781729,12.75));
#7322=CARTESIAN_POINT('Ctrl Pts',(3.02934403325601,9.4502236812248,-3.75));
#7323=CARTESIAN_POINT('Ctrl Pts',(3.02934403325601,9.4502236812248,12.75));
#7324=CARTESIAN_POINT('Ctrl Pts',(2.98420577513996,9.4109471173216,-3.75));
#7325=CARTESIAN_POINT('Ctrl Pts',(2.98420577513996,9.4109471173216,12.75));
#7326=CARTESIAN_POINT('Ctrl Pts',(2.9396747031485,9.3712871143499,-3.75));
#7327=CARTESIAN_POINT('Ctrl Pts',(2.9396747031485,9.3712871143499,12.75));
#7328=CARTESIAN_POINT('Ctrl Pts',(2.89575377593938,9.33124817395869,-3.75));
#7329=CARTESIAN_POINT('Ctrl Pts',(2.89575377593938,9.33124817395869,12.75));
#7330=CARTESIAN_POINT('Ctrl Pts',(2.8524523828002,9.29083237315974,-3.75));
#7331=CARTESIAN_POINT('Ctrl Pts',(2.8524523828002,9.29083237315974,12.75));
#7332=CARTESIAN_POINT('Ctrl Pts',(2.8097905150733,9.2500377269296,-3.75));
#7333=CARTESIAN_POINT('Ctrl Pts',(2.8097905150733,9.2500377269296,12.75));
#7334=CARTESIAN_POINT('Ctrl Pts',(2.76780196452137,9.20885693589776,-3.75));
#7335=CARTESIAN_POINT('Ctrl Pts',(2.76780196452137,9.20885693589776,12.75));
#7336=CARTESIAN_POINT('Ctrl Pts',(2.72652481622916,9.16728115317076,-3.75));
#7337=CARTESIAN_POINT('Ctrl Pts',(2.72652481622916,9.16728115317076,12.75));
#7338=CARTESIAN_POINT('Ctrl Pts',(2.68599232523134,9.12530360007999,-3.75));
#7339=CARTESIAN_POINT('Ctrl Pts',(2.68599232523134,9.12530360007999,12.75));
#7340=CARTESIAN_POINT('Ctrl Pts',(2.64622438896052,9.08292294803309,-3.75));
#7341=CARTESIAN_POINT('Ctrl Pts',(2.64622438896052,9.08292294803309,12.75));
#7342=CARTESIAN_POINT('Ctrl Pts',(2.60721699951879,9.0401474973841,-3.75));
#7343=CARTESIAN_POINT('Ctrl Pts',(2.60721699951879,9.0401474973841,12.75));
#7344=CARTESIAN_POINT('Ctrl Pts',(2.56893767747319,8.99699699918147,-3.75));
#7345=CARTESIAN_POINT('Ctrl Pts',(2.56893767747319,8.99699699918147,12.75));
#7346=CARTESIAN_POINT('Ctrl Pts',(2.53134978004338,8.95349309713545,-3.75));
#7347=CARTESIAN_POINT('Ctrl Pts',(2.53134978004338,8.95349309713545,12.75));
#7348=CARTESIAN_POINT('Ctrl Pts',(2.4944346415182,8.90965062344541,-3.75));
#7349=CARTESIAN_POINT('Ctrl Pts',(2.4944346415182,8.90965062344541,12.75));
#7350=CARTESIAN_POINT('Ctrl Pts',(2.45821141167119,8.86546980570045,-3.75));
#7351=CARTESIAN_POINT('Ctrl Pts',(2.45821141167119,8.86546980570045,12.75));
#7352=CARTESIAN_POINT('Ctrl Pts',(2.42276538248091,8.82092512134556,-3.75));
#7353=CARTESIAN_POINT('Ctrl Pts',(2.42276538248091,8.82092512134556,12.75));
#7354=CARTESIAN_POINT('Ctrl Pts',(2.38824857383288,8.77596511266658,-3.75));
#7355=CARTESIAN_POINT('Ctrl Pts',(2.38824857383288,8.77596511266658,12.75));
#7356=CARTESIAN_POINT('Ctrl Pts',(2.35482147675118,8.73053548487858,-3.75));
#7357=CARTESIAN_POINT('Ctrl Pts',(2.35482147675118,8.73053548487858,12.75));
#7358=CARTESIAN_POINT('Ctrl Pts',(2.32260171926006,8.68459942442028,-3.75));
#7359=CARTESIAN_POINT('Ctrl Pts',(2.32260171926006,8.68459942442028,12.75));
#7360=CARTESIAN_POINT('Ctrl Pts',(2.29162050823336,8.63815494571075,-3.75));
#7361=CARTESIAN_POINT('Ctrl Pts',(2.29162050823336,8.63815494571075,12.75));
#7362=CARTESIAN_POINT('Ctrl Pts',(2.26174990860571,8.59126351952004,-3.75));
#7363=CARTESIAN_POINT('Ctrl Pts',(2.26174990860571,8.59126351952004,12.75));
#7364=CARTESIAN_POINT('Ctrl Pts',(2.23274297834755,8.54403497990068,-3.75));
#7365=CARTESIAN_POINT('Ctrl Pts',(2.23274297834755,8.54403497990068,12.75));
#7366=CARTESIAN_POINT('Ctrl Pts',(2.20438215159743,8.49657041043195,-3.75));
#7367=CARTESIAN_POINT('Ctrl Pts',(2.20438215159743,8.49657041043195,12.75));
#7368=CARTESIAN_POINT('Ctrl Pts',(2.17660700812682,8.44891314968814,-3.75));
#7369=CARTESIAN_POINT('Ctrl Pts',(2.17660700812682,8.44891314968814,12.75));
#7370=CARTESIAN_POINT('Ctrl Pts',(2.1496314108288,8.40100363162428,-3.75));
#7371=CARTESIAN_POINT('Ctrl Pts',(2.1496314108288,8.40100363162428,12.75));
#7372=CARTESIAN_POINT('Ctrl Pts',(2.12411443763999,8.35261410600662,-3.75));
#7373=CARTESIAN_POINT('Ctrl Pts',(2.12411443763999,8.35261410600662,12.75));
#7374=CARTESIAN_POINT('Ctrl Pts',(2.10101049300138,8.3034037182712,-3.75));
#7375=CARTESIAN_POINT('Ctrl Pts',(2.10101049300138,8.3034037182712,12.75));
#7376=CARTESIAN_POINT('Ctrl Pts',(2.08524426770063,8.26309465918435,-3.75));
#7377=CARTESIAN_POINT('Ctrl Pts',(2.08524426770063,8.26309465918435,12.75));
#7378=CARTESIAN_POINT('Ctrl Pts',(2.07530073900944,8.23220544002367,-3.75));
#7379=CARTESIAN_POINT('Ctrl Pts',(2.07530073900944,8.23220544002367,12.75));
#7380=CARTESIAN_POINT('Ctrl Pts',(2.06955313972063,8.21130388109186,-3.75));
#7381=CARTESIAN_POINT('Ctrl Pts',(2.06955313972063,8.21130388109186,12.75));
#7382=CARTESIAN_POINT('Ctrl Pts',(2.066899701215,8.20077591276801,-3.75));
#7383=CARTESIAN_POINT('Ctrl Pts',(2.066899701215,8.20077591276801,12.75));
#7384=CARTESIAN_POINT('',(5.3791293750062,10.7268339768519,-1.));
#7385=CARTESIAN_POINT('Ctrl Pts',(5.37912937500617,10.726833976852,-1.));
#7386=CARTESIAN_POINT('Ctrl Pts',(5.36620715918271,10.7225897134991,-1.));
#7387=CARTESIAN_POINT('Ctrl Pts',(5.34039795525198,10.714055870666,-1.));
#7388=CARTESIAN_POINT('Ctrl Pts',(5.30178983253176,10.7011191580639,-1.));
#7389=CARTESIAN_POINT('Ctrl Pts',(5.25052377191006,10.6835982206291,-1.));
#7390=CARTESIAN_POINT('Ctrl Pts',(5.18679427410258,10.661243291145,-1.));
#7391=CARTESIAN_POINT('Ctrl Pts',(5.12341919820984,10.638434168447,-1.));
#7392=CARTESIAN_POINT('Ctrl Pts',(5.06040071098369,10.6151706715837,-1.));
#7393=CARTESIAN_POINT('Ctrl Pts',(4.99774193408264,10.5914530920551,-1.));
#7394=CARTESIAN_POINT('Ctrl Pts',(4.93544714999767,10.5672824880187,-1.));
#7395=CARTESIAN_POINT('Ctrl Pts',(4.87352158939686,10.5426605691059,-1.));
#7396=CARTESIAN_POINT('Ctrl Pts',(4.81197108362035,10.5175894490106,-1.));
#7397=CARTESIAN_POINT('Ctrl Pts',(4.7508017470924,10.4920714379865,-1.));
#7398=CARTESIAN_POINT('Ctrl Pts',(4.69001967404875,10.4661088391609,-1.));
#7399=CARTESIAN_POINT('Ctrl Pts',(4.62963055491846,10.4397037052484,-1.));
#7400=CARTESIAN_POINT('Ctrl Pts',(4.56963961142454,10.4128577818052,-1.));
#7401=CARTESIAN_POINT('Ctrl Pts',(4.5100518320603,10.3855726289458,-1.));
#7402=CARTESIAN_POINT('Ctrl Pts',(4.45087212698485,10.3578496987941,-1.));
#7403=CARTESIAN_POINT('Ctrl Pts',(4.39210550098945,10.3296904287044,-1.));
#7404=CARTESIAN_POINT('Ctrl Pts',(4.33375724408484,10.3010963438997,-1.));
#7405=CARTESIAN_POINT('Ctrl Pts',(4.27583301771353,10.272069116189,-1.));
#7406=CARTESIAN_POINT('Ctrl Pts',(4.21833871177567,10.2426105188232,-1.));
#7407=CARTESIAN_POINT('Ctrl Pts',(4.16128034451962,10.2127224064663,-1.));
#7408=CARTESIAN_POINT('Ctrl Pts',(4.10466394929486,10.1824066879509,-1.));
#7409=CARTESIAN_POINT('Ctrl Pts',(4.04849544744087,10.1516653064199,-1.));
#7410=CARTESIAN_POINT('Ctrl Pts',(3.99278057289046,10.1205002164952,-1.));
#7411=CARTESIAN_POINT('Ctrl Pts',(3.93752506012707,10.0889133486827,-1.));
#7412=CARTESIAN_POINT('Ctrl Pts',(3.88273479532263,10.056906577166,-1.));
#7413=CARTESIAN_POINT('Ctrl Pts',(3.82841597408715,10.0244816905709,-1.));
#7414=CARTESIAN_POINT('Ctrl Pts',(3.77457526401004,9.99164036147395,-1.));
#7415=CARTESIAN_POINT('Ctrl Pts',(3.72121993173636,9.95838412799172,-1.));
#7416=CARTESIAN_POINT('Ctrl Pts',(3.66835753420625,9.92471449880883,-1.));
#7417=CARTESIAN_POINT('Ctrl Pts',(3.61599563628969,9.89063305253546,-1.));
#7418=CARTESIAN_POINT('Ctrl Pts',(3.56414151726151,9.85614154137781,-1.));
#7419=CARTESIAN_POINT('Ctrl Pts',(3.51280187273295,9.8212419982557,-1.));
#7420=CARTESIAN_POINT('Ctrl Pts',(3.46198252886957,9.78593684022037,-1.));
#7421=CARTESIAN_POINT('Ctrl Pts',(3.41168916880891,9.75022858813702,-1.));
#7422=CARTESIAN_POINT('Ctrl Pts',(3.36192803839197,9.7141195953304,-1.));
#7423=CARTESIAN_POINT('Ctrl Pts',(3.31270665744062,9.67761177523123,-1.));
#7424=CARTESIAN_POINT('Ctrl Pts',(3.26403452382222,9.64070633286081,-1.));
#7425=CARTESIAN_POINT('Ctrl Pts',(3.2159238260067,9.60340349406962,-1.));
#7426=CARTESIAN_POINT('Ctrl Pts',(3.16838785383004,9.56570313257491,-1.));
#7427=CARTESIAN_POINT('Ctrl Pts',(3.12143939300699,9.52760540436562,-1.));
#7428=CARTESIAN_POINT('Ctrl Pts',(3.07508913212204,9.4891113781729,-1.));
#7429=CARTESIAN_POINT('Ctrl Pts',(3.02934403325601,9.4502236812248,-1.));
#7430=CARTESIAN_POINT('Ctrl Pts',(2.98420577513996,9.4109471173216,-1.));
#7431=CARTESIAN_POINT('Ctrl Pts',(2.9396747031485,9.3712871143499,-1.));
#7432=CARTESIAN_POINT('Ctrl Pts',(2.89575377593938,9.33124817395869,-1.));
#7433=CARTESIAN_POINT('Ctrl Pts',(2.8524523828002,9.29083237315974,-1.));
#7434=CARTESIAN_POINT('Ctrl Pts',(2.8097905150733,9.2500377269296,-1.));
#7435=CARTESIAN_POINT('Ctrl Pts',(2.76780196452137,9.20885693589776,-1.));
#7436=CARTESIAN_POINT('Ctrl Pts',(2.72652481622916,9.16728115317076,-1.));
#7437=CARTESIAN_POINT('Ctrl Pts',(2.68599232523134,9.12530360007999,-1.));
#7438=CARTESIAN_POINT('Ctrl Pts',(2.64622438896052,9.08292294803309,-1.));
#7439=CARTESIAN_POINT('Ctrl Pts',(2.60721699951879,9.0401474973841,-1.));
#7440=CARTESIAN_POINT('Ctrl Pts',(2.56893767747319,8.99699699918147,-1.));
#7441=CARTESIAN_POINT('Ctrl Pts',(2.53134978004338,8.95349309713545,-1.));
#7442=CARTESIAN_POINT('Ctrl Pts',(2.4944346415182,8.90965062344541,-1.));
#7443=CARTESIAN_POINT('Ctrl Pts',(2.45821141167119,8.86546980570045,-1.));
#7444=CARTESIAN_POINT('Ctrl Pts',(2.42276538248091,8.82092512134556,-1.));
#7445=CARTESIAN_POINT('Ctrl Pts',(2.38824857383288,8.77596511266658,-1.));
#7446=CARTESIAN_POINT('Ctrl Pts',(2.35482147675118,8.73053548487858,-1.));
#7447=CARTESIAN_POINT('Ctrl Pts',(2.32260171926006,8.68459942442028,-1.));
#7448=CARTESIAN_POINT('Ctrl Pts',(2.29162050823336,8.63815494571075,-1.));
#7449=CARTESIAN_POINT('Ctrl Pts',(2.26174990860571,8.59126351952004,-1.));
#7450=CARTESIAN_POINT('Ctrl Pts',(2.23274297834755,8.54403497990068,-1.));
#7451=CARTESIAN_POINT('Ctrl Pts',(2.20438215159743,8.49657041043195,-1.));
#7452=CARTESIAN_POINT('Ctrl Pts',(2.17660700812682,8.44891314968814,-1.));
#7453=CARTESIAN_POINT('Ctrl Pts',(2.1496314108288,8.40100363162428,-1.));
#7454=CARTESIAN_POINT('Ctrl Pts',(2.12411443763999,8.35261410600662,-1.));
#7455=CARTESIAN_POINT('Ctrl Pts',(2.10101049300138,8.3034037182712,-1.));
#7456=CARTESIAN_POINT('Ctrl Pts',(2.08524426770063,8.26309465918435,-1.));
#7457=CARTESIAN_POINT('Ctrl Pts',(2.07530073900944,8.23220544002367,-1.));
#7458=CARTESIAN_POINT('Ctrl Pts',(2.06955313972063,8.21130388109186,-1.));
#7459=CARTESIAN_POINT('Ctrl Pts',(2.066899701215,8.20077591276801,-1.));
#7460=CARTESIAN_POINT('',(5.3791293750062,10.7268339768519,6.));
#7461=CARTESIAN_POINT('Ctrl Pts',(5.37912937500617,10.726833976852,6.));
#7462=CARTESIAN_POINT('Ctrl Pts',(5.36620715918271,10.7225897134991,6.));
#7463=CARTESIAN_POINT('Ctrl Pts',(5.34039795525198,10.714055870666,6.));
#7464=CARTESIAN_POINT('Ctrl Pts',(5.30178983253176,10.7011191580639,6.));
#7465=CARTESIAN_POINT('Ctrl Pts',(5.25052377191006,10.6835982206291,6.));
#7466=CARTESIAN_POINT('Ctrl Pts',(5.18679427410258,10.661243291145,6.));
#7467=CARTESIAN_POINT('Ctrl Pts',(5.12341919820984,10.638434168447,6.));
#7468=CARTESIAN_POINT('Ctrl Pts',(5.06040071098369,10.6151706715837,6.));
#7469=CARTESIAN_POINT('Ctrl Pts',(4.99774193408264,10.5914530920551,6.));
#7470=CARTESIAN_POINT('Ctrl Pts',(4.93544714999767,10.5672824880187,6.));
#7471=CARTESIAN_POINT('Ctrl Pts',(4.87352158939686,10.5426605691059,6.));
#7472=CARTESIAN_POINT('Ctrl Pts',(4.81197108362035,10.5175894490106,6.));
#7473=CARTESIAN_POINT('Ctrl Pts',(4.7508017470924,10.4920714379865,6.));
#7474=CARTESIAN_POINT('Ctrl Pts',(4.69001967404875,10.4661088391609,6.));
#7475=CARTESIAN_POINT('Ctrl Pts',(4.62963055491846,10.4397037052484,6.));
#7476=CARTESIAN_POINT('Ctrl Pts',(4.56963961142454,10.4128577818052,6.));
#7477=CARTESIAN_POINT('Ctrl Pts',(4.5100518320603,10.3855726289458,6.));
#7478=CARTESIAN_POINT('Ctrl Pts',(4.45087212698485,10.3578496987941,6.));
#7479=CARTESIAN_POINT('Ctrl Pts',(4.39210550098945,10.3296904287044,6.));
#7480=CARTESIAN_POINT('Ctrl Pts',(4.33375724408484,10.3010963438997,6.));
#7481=CARTESIAN_POINT('Ctrl Pts',(4.27583301771353,10.272069116189,6.));
#7482=CARTESIAN_POINT('Ctrl Pts',(4.21833871177567,10.2426105188232,6.));
#7483=CARTESIAN_POINT('Ctrl Pts',(4.16128034451962,10.2127224064663,6.));
#7484=CARTESIAN_POINT('Ctrl Pts',(4.10466394929486,10.1824066879509,6.));
#7485=CARTESIAN_POINT('Ctrl Pts',(4.04849544744087,10.1516653064199,6.));
#7486=CARTESIAN_POINT('Ctrl Pts',(3.99278057289046,10.1205002164952,6.));
#7487=CARTESIAN_POINT('Ctrl Pts',(3.93752506012707,10.0889133486827,6.));
#7488=CARTESIAN_POINT('Ctrl Pts',(3.88273479532263,10.056906577166,6.));
#7489=CARTESIAN_POINT('Ctrl Pts',(3.82841597408715,10.0244816905709,6.));
#7490=CARTESIAN_POINT('Ctrl Pts',(3.77457526401004,9.99164036147395,6.));
#7491=CARTESIAN_POINT('Ctrl Pts',(3.72121993173636,9.95838412799172,6.));
#7492=CARTESIAN_POINT('Ctrl Pts',(3.66835753420625,9.92471449880883,6.));
#7493=CARTESIAN_POINT('Ctrl Pts',(3.61599563628969,9.89063305253546,6.));
#7494=CARTESIAN_POINT('Ctrl Pts',(3.56414151726151,9.85614154137781,6.));
#7495=CARTESIAN_POINT('Ctrl Pts',(3.51280187273295,9.8212419982557,6.));
#7496=CARTESIAN_POINT('Ctrl Pts',(3.46198252886957,9.78593684022037,6.));
#7497=CARTESIAN_POINT('Ctrl Pts',(3.41168916880891,9.75022858813702,6.));
#7498=CARTESIAN_POINT('Ctrl Pts',(3.36192803839197,9.7141195953304,6.));
#7499=CARTESIAN_POINT('Ctrl Pts',(3.31270665744062,9.67761177523123,6.));
#7500=CARTESIAN_POINT('Ctrl Pts',(3.26403452382222,9.64070633286081,6.));
#7501=CARTESIAN_POINT('Ctrl Pts',(3.2159238260067,9.60340349406962,6.));
#7502=CARTESIAN_POINT('Ctrl Pts',(3.16838785383004,9.56570313257491,6.));
#7503=CARTESIAN_POINT('Ctrl Pts',(3.12143939300699,9.52760540436562,6.));
#7504=CARTESIAN_POINT('Ctrl Pts',(3.07508913212204,9.4891113781729,6.));
#7505=CARTESIAN_POINT('Ctrl Pts',(3.02934403325601,9.4502236812248,6.));
#7506=CARTESIAN_POINT('Ctrl Pts',(2.98420577513996,9.4109471173216,6.));
#7507=CARTESIAN_POINT('Ctrl Pts',(2.9396747031485,9.3712871143499,6.));
#7508=CARTESIAN_POINT('Ctrl Pts',(2.89575377593938,9.33124817395869,6.));
#7509=CARTESIAN_POINT('Ctrl Pts',(2.8524523828002,9.29083237315974,6.));
#7510=CARTESIAN_POINT('Ctrl Pts',(2.8097905150733,9.2500377269296,6.));
#7511=CARTESIAN_POINT('Ctrl Pts',(2.76780196452137,9.20885693589776,6.));
#7512=CARTESIAN_POINT('Ctrl Pts',(2.72652481622916,9.16728115317076,6.));
#7513=CARTESIAN_POINT('Ctrl Pts',(2.68599232523134,9.12530360007999,6.));
#7514=CARTESIAN_POINT('Ctrl Pts',(2.64622438896052,9.08292294803309,6.));
#7515=CARTESIAN_POINT('Ctrl Pts',(2.60721699951879,9.0401474973841,6.));
#7516=CARTESIAN_POINT('Ctrl Pts',(2.56893767747319,8.99699699918147,6.));
#7517=CARTESIAN_POINT('Ctrl Pts',(2.53134978004338,8.95349309713545,6.));
#7518=CARTESIAN_POINT('Ctrl Pts',(2.4944346415182,8.90965062344541,6.));
#7519=CARTESIAN_POINT('Ctrl Pts',(2.45821141167119,8.86546980570045,6.));
#7520=CARTESIAN_POINT('Ctrl Pts',(2.42276538248091,8.82092512134556,6.));
#7521=CARTESIAN_POINT('Ctrl Pts',(2.38824857383288,8.77596511266658,6.));
#7522=CARTESIAN_POINT('Ctrl Pts',(2.35482147675118,8.73053548487858,6.));
#7523=CARTESIAN_POINT('Ctrl Pts',(2.32260171926006,8.68459942442028,6.));
#7524=CARTESIAN_POINT('Ctrl Pts',(2.29162050823336,8.63815494571075,6.));
#7525=CARTESIAN_POINT('Ctrl Pts',(2.26174990860571,8.59126351952004,6.));
#7526=CARTESIAN_POINT('Ctrl Pts',(2.23274297834755,8.54403497990068,6.));
#7527=CARTESIAN_POINT('Ctrl Pts',(2.20438215159743,8.49657041043195,6.));
#7528=CARTESIAN_POINT('Ctrl Pts',(2.17660700812682,8.44891314968814,6.));
#7529=CARTESIAN_POINT('Ctrl Pts',(2.1496314108288,8.40100363162428,6.));
#7530=CARTESIAN_POINT('Ctrl Pts',(2.12411443763999,8.35261410600662,6.));
#7531=CARTESIAN_POINT('Ctrl Pts',(2.10101049300138,8.3034037182712,6.));
#7532=CARTESIAN_POINT('Ctrl Pts',(2.08524426770063,8.26309465918435,6.));
#7533=CARTESIAN_POINT('Ctrl Pts',(2.07530073900944,8.23220544002367,6.));
#7534=CARTESIAN_POINT('Ctrl Pts',(2.06955313972063,8.21130388109186,6.));
#7535=CARTESIAN_POINT('Ctrl Pts',(2.066899701215,8.20077591276801,6.));
#7536=CARTESIAN_POINT('',(5.3791293750062,10.7268339768519,0.));
#7537=CARTESIAN_POINT('Origin',(1.99840144432528E-13,3.46133283549042E-13,
0.));
#7538=CARTESIAN_POINT('',(6.60014603862877,10.0218796774244,-1.));
#7539=CARTESIAN_POINT('Origin',(1.99840144432528E-13,3.46133283549042E-13,
-1.));
#7540=CARTESIAN_POINT('',(6.60014603862877,10.0218796774244,6.));
#7541=CARTESIAN_POINT('Origin',(1.99840144432528E-13,3.46133283549042E-13,
6.));
#7542=CARTESIAN_POINT('',(6.60014603862877,10.0218796774244,0.));
#7543=CARTESIAN_POINT('Ctrl Pts',(6.06863042059311,5.89037560471066,-3.75));
#7544=CARTESIAN_POINT('Ctrl Pts',(6.06863042059311,5.89037560471066,12.75));
#7545=CARTESIAN_POINT('Ctrl Pts',(6.07642118935899,5.89793753402584,-3.75));
#7546=CARTESIAN_POINT('Ctrl Pts',(6.07642118935899,5.89793753402584,12.75));
#7547=CARTESIAN_POINT('Ctrl Pts',(6.09164867072823,5.91336588048663,-3.75));
#7548=CARTESIAN_POINT('Ctrl Pts',(6.09164867072823,5.91336588048663,12.75));
#7549=CARTESIAN_POINT('Ctrl Pts',(6.11342775487885,5.93742183851679,-3.75));
#7550=CARTESIAN_POINT('Ctrl Pts',(6.11342775487885,5.93742183851679,12.75));
#7551=CARTESIAN_POINT('Ctrl Pts',(6.14045331140034,5.97123031969246,-3.75));
#7552=CARTESIAN_POINT('Ctrl Pts',(6.14045331140034,5.97123031969246,12.75));
#7553=CARTESIAN_POINT('Ctrl Pts',(6.17151878498999,6.01584411654484,-3.75));
#7554=CARTESIAN_POINT('Ctrl Pts',(6.17151878498999,6.01584411654484,12.75));
#7555=CARTESIAN_POINT('Ctrl Pts',(6.20066685685755,6.06213722636286,-3.75));
#7556=CARTESIAN_POINT('Ctrl Pts',(6.20066685685755,6.06213722636286,12.75));
#7557=CARTESIAN_POINT('Ctrl Pts',(6.22866991793492,6.10945353793713,-3.75));
#7558=CARTESIAN_POINT('Ctrl Pts',(6.22866991793492,6.10945353793713,12.75));
#7559=CARTESIAN_POINT('Ctrl Pts',(6.25605474467853,6.15733614814835,-3.75));
#7560=CARTESIAN_POINT('Ctrl Pts',(6.25605474467853,6.15733614814835,12.75));
#7561=CARTESIAN_POINT('Ctrl Pts',(6.28297985424308,6.20562962932065,-3.75));
#7562=CARTESIAN_POINT('Ctrl Pts',(6.28297985424308,6.20562962932065,12.75));
#7563=CARTESIAN_POINT('Ctrl Pts',(6.30937750420801,6.2543646376197,-3.75));
#7564=CARTESIAN_POINT('Ctrl Pts',(6.30937750420801,6.2543646376197,12.75));
#7565=CARTESIAN_POINT('Ctrl Pts',(6.33505137069502,6.30367904881887,-3.75));
#7566=CARTESIAN_POINT('Ctrl Pts',(6.33505137069502,6.30367904881887,12.75));
#7567=CARTESIAN_POINT('Ctrl Pts',(6.35978286360965,6.35373180396277,-3.75));
#7568=CARTESIAN_POINT('Ctrl Pts',(6.35978286360965,6.35373180396277,12.75));
#7569=CARTESIAN_POINT('Ctrl Pts',(6.38345478017076,6.40460296268299,-3.75));
#7570=CARTESIAN_POINT('Ctrl Pts',(6.38345478017076,6.40460296268299,12.75));
#7571=CARTESIAN_POINT('Ctrl Pts',(6.40608444337878,6.45626649182452,-3.75));
#7572=CARTESIAN_POINT('Ctrl Pts',(6.40608444337878,6.45626649182452,12.75));
#7573=CARTESIAN_POINT('Ctrl Pts',(6.42776254872513,6.50863892931076,-3.75));
#7574=CARTESIAN_POINT('Ctrl Pts',(6.42776254872513,6.50863892931076,12.75));
#7575=CARTESIAN_POINT('Ctrl Pts',(6.44861636238489,6.56160843323028,-3.75));
#7576=CARTESIAN_POINT('Ctrl Pts',(6.44861636238489,6.56160843323028,12.75));
#7577=CARTESIAN_POINT('Ctrl Pts',(6.46876645798849,6.6150690793574,-3.75));
#7578=CARTESIAN_POINT('Ctrl Pts',(6.46876645798849,6.6150690793574,12.75));
#7579=CARTESIAN_POINT('Ctrl Pts',(6.48827758470623,6.66895976394944,-3.75));
#7580=CARTESIAN_POINT('Ctrl Pts',(6.48827758470623,6.66895976394944,12.75));
#7581=CARTESIAN_POINT('Ctrl Pts',(6.50715912032692,6.72326378902151,-3.75));
#7582=CARTESIAN_POINT('Ctrl Pts',(6.50715912032692,6.72326378902151,12.75));
#7583=CARTESIAN_POINT('Ctrl Pts',(6.52538888693356,6.77798990345396,-3.75));
#7584=CARTESIAN_POINT('Ctrl Pts',(6.52538888693356,6.77798990345396,12.75));
#7585=CARTESIAN_POINT('Ctrl Pts',(6.54292981913304,6.83315901897031,-3.75));
#7586=CARTESIAN_POINT('Ctrl Pts',(6.54292981913304,6.83315901897031,12.75));
#7587=CARTESIAN_POINT('Ctrl Pts',(6.5597485722992,6.88878938806037,-3.75));
#7588=CARTESIAN_POINT('Ctrl Pts',(6.5597485722992,6.88878938806037,12.75));
#7589=CARTESIAN_POINT('Ctrl Pts',(6.5758359541656,6.94488033148853,-3.75));
#7590=CARTESIAN_POINT('Ctrl Pts',(6.5758359541656,6.94488033148853,12.75));
#7591=CARTESIAN_POINT('Ctrl Pts',(6.5912030640433,7.00141528186886,-3.75));
#7592=CARTESIAN_POINT('Ctrl Pts',(6.5912030640433,7.00141528186886,12.75));
#7593=CARTESIAN_POINT('Ctrl Pts',(6.60587239994885,7.05836882883084,-3.75));
#7594=CARTESIAN_POINT('Ctrl Pts',(6.60587239994885,7.05836882883084,12.75));
#7595=CARTESIAN_POINT('Ctrl Pts',(6.61987066605911,7.11571241317029,-3.75));
#7596=CARTESIAN_POINT('Ctrl Pts',(6.61987066605911,7.11571241317029,12.75));
#7597=CARTESIAN_POINT('Ctrl Pts',(6.63322107969569,7.17342042004755,-3.75));
#7598=CARTESIAN_POINT('Ctrl Pts',(6.63322107969569,7.17342042004755,12.75));
#7599=CARTESIAN_POINT('Ctrl Pts',(6.64593535561053,7.23147652896403,-3.75));
#7600=CARTESIAN_POINT('Ctrl Pts',(6.64593535561053,7.23147652896403,12.75));
#7601=CARTESIAN_POINT('Ctrl Pts',(6.65801638970246,7.28987157005223,-3.75));
#7602=CARTESIAN_POINT('Ctrl Pts',(6.65801638970246,7.28987157005223,12.75));
#7603=CARTESIAN_POINT('Ctrl Pts',(6.66946176275797,7.34860073021491,-3.75));
#7604=CARTESIAN_POINT('Ctrl Pts',(6.66946176275797,7.34860073021491,12.75));
#7605=CARTESIAN_POINT('Ctrl Pts',(6.68026694677668,7.40766099640557,-3.75));
#7606=CARTESIAN_POINT('Ctrl Pts',(6.68026694677668,7.40766099640557,12.75));
#7607=CARTESIAN_POINT('Ctrl Pts',(6.69042862091104,7.46704851290034,-3.75));
#7608=CARTESIAN_POINT('Ctrl Pts',(6.69042862091104,7.46704851290034,12.75));
#7609=CARTESIAN_POINT('Ctrl Pts',(6.69994799095524,7.52675593674632,-3.75));
#7610=CARTESIAN_POINT('Ctrl Pts',(6.69994799095524,7.52675593674632,12.75));
#7611=CARTESIAN_POINT('Ctrl Pts',(6.70882947565318,7.58677347699226,-3.75));
#7612=CARTESIAN_POINT('Ctrl Pts',(6.70882947565318,7.58677347699226,12.75));
#7613=CARTESIAN_POINT('Ctrl Pts',(6.71707933277187,7.64708998288989,-3.75));
#7614=CARTESIAN_POINT('Ctrl Pts',(6.71707933277187,7.64708998288989,12.75));
#7615=CARTESIAN_POINT('Ctrl Pts',(6.72470431659336,7.70769400824503,-3.75));
#7616=CARTESIAN_POINT('Ctrl Pts',(6.72470431659336,7.70769400824503,12.75));
#7617=CARTESIAN_POINT('Ctrl Pts',(6.73171032576036,7.76857488460783,-3.75));
#7618=CARTESIAN_POINT('Ctrl Pts',(6.73171032576036,7.76857488460783,12.75));
#7619=CARTESIAN_POINT('Ctrl Pts',(6.73810106562749,7.82972378407324,-3.75));
#7620=CARTESIAN_POINT('Ctrl Pts',(6.73810106562749,7.82972378407324,12.75));
#7621=CARTESIAN_POINT('Ctrl Pts',(6.74387863902608,7.89113323756912,-3.75));
#7622=CARTESIAN_POINT('Ctrl Pts',(6.74387863902608,7.89113323756912,12.75));
#7623=CARTESIAN_POINT('Ctrl Pts',(6.7490441308376,7.95279665937614,-3.75));
#7624=CARTESIAN_POINT('Ctrl Pts',(6.7490441308376,7.95279665937614,12.75));
#7625=CARTESIAN_POINT('Ctrl Pts',(6.75359819949754,8.01470786732018,-3.75));
#7626=CARTESIAN_POINT('Ctrl Pts',(6.75359819949754,8.01470786732018,12.75));
#7627=CARTESIAN_POINT('Ctrl Pts',(6.75754166486089,8.07686060726827,-3.75));
#7628=CARTESIAN_POINT('Ctrl Pts',(6.75754166486089,8.07686060726827,12.75));
#7629=CARTESIAN_POINT('Ctrl Pts',(6.76087611417306,8.13924806419107,-3.75));
#7630=CARTESIAN_POINT('Ctrl Pts',(6.76087611417306,8.13924806419107,12.75));
#7631=CARTESIAN_POINT('Ctrl Pts',(6.7636036696164,8.20186305794855,-3.75));
#7632=CARTESIAN_POINT('Ctrl Pts',(6.7636036696164,8.20186305794855,12.75));
#7633=CARTESIAN_POINT('Ctrl Pts',(6.76572674650935,8.26469824786602,-3.75));
#7634=CARTESIAN_POINT('Ctrl Pts',(6.76572674650935,8.26469824786602,12.75));
#7635=CARTESIAN_POINT('Ctrl Pts',(6.76724781676282,8.32774633509908,-3.75));
#7636=CARTESIAN_POINT('Ctrl Pts',(6.76724781676282,8.32774633509908,12.75));
#7637=CARTESIAN_POINT('Ctrl Pts',(6.76816918165128,8.39100025749018,-3.75));
#7638=CARTESIAN_POINT('Ctrl Pts',(6.76816918165128,8.39100025749018,12.75));
#7639=CARTESIAN_POINT('Ctrl Pts',(6.76849272647565,8.45445340444926,-3.75));
#7640=CARTESIAN_POINT('Ctrl Pts',(6.76849272647565,8.45445340444926,12.75));
#7641=CARTESIAN_POINT('Ctrl Pts',(6.76822000004555,8.51809951610774,-3.75));
#7642=CARTESIAN_POINT('Ctrl Pts',(6.76822000004555,8.51809951610774,12.75));
#7643=CARTESIAN_POINT('Ctrl Pts',(6.76735232235635,8.58193255779939,-3.75));
#7644=CARTESIAN_POINT('Ctrl Pts',(6.76735232235635,8.58193255779939,12.75));
#7645=CARTESIAN_POINT('Ctrl Pts',(6.76589088878265,8.64594659806298,-3.75));
#7646=CARTESIAN_POINT('Ctrl Pts',(6.76589088878265,8.64594659806298,12.75));
#7647=CARTESIAN_POINT('Ctrl Pts',(6.76383687353853,8.71013569385599,-3.75));
#7648=CARTESIAN_POINT('Ctrl Pts',(6.76383687353853,8.71013569385599,12.75));
#7649=CARTESIAN_POINT('Ctrl Pts',(6.76119155448275,8.77449374557664,-3.75));
#7650=CARTESIAN_POINT('Ctrl Pts',(6.76119155448275,8.77449374557664,12.75));
#7651=CARTESIAN_POINT('Ctrl Pts',(6.7579562951925,8.83901457377471,-3.75));
#7652=CARTESIAN_POINT('Ctrl Pts',(6.7579562951925,8.83901457377471,12.75));
#7653=CARTESIAN_POINT('Ctrl Pts',(6.75413249860576,8.90369203916218,-3.75));
#7654=CARTESIAN_POINT('Ctrl Pts',(6.75413249860576,8.90369203916218,12.75));
#7655=CARTESIAN_POINT('Ctrl Pts',(6.74972157399229,8.96852015431046,-3.75));
#7656=CARTESIAN_POINT('Ctrl Pts',(6.74972157399229,8.96852015431046,12.75));
#7657=CARTESIAN_POINT('Ctrl Pts',(6.74472490424422,9.03349318036198,-3.75));
#7658=CARTESIAN_POINT('Ctrl Pts',(6.74472490424422,9.03349318036198,12.75));
#7659=CARTESIAN_POINT('Ctrl Pts',(6.73914381348523,9.09860577342165,-3.75));
#7660=CARTESIAN_POINT('Ctrl Pts',(6.73914381348523,9.09860577342165,12.75));
#7661=CARTESIAN_POINT('Ctrl Pts',(6.73297955932548,9.16385288053588,-3.75));
#7662=CARTESIAN_POINT('Ctrl Pts',(6.73297955932548,9.16385288053588,12.75));
#7663=CARTESIAN_POINT('Ctrl Pts',(6.72623333926846,9.22922952332026,-3.75));
#7664=CARTESIAN_POINT('Ctrl Pts',(6.72623333926846,9.22922952332026,12.75));
#7665=CARTESIAN_POINT('Ctrl Pts',(6.71890629646187,9.2947306015555,-3.75));
#7666=CARTESIAN_POINT('Ctrl Pts',(6.71890629646187,9.2947306015555,12.75));
#7667=CARTESIAN_POINT('Ctrl Pts',(6.71099953007124,9.36035072031876,-3.75));
#7668=CARTESIAN_POINT('Ctrl Pts',(6.71099953007124,9.36035072031876,12.75));
#7669=CARTESIAN_POINT('Ctrl Pts',(6.70251410760819,9.42608392519666,-3.75));
#7670=CARTESIAN_POINT('Ctrl Pts',(6.70251410760819,9.42608392519666,12.75));
#7671=CARTESIAN_POINT('Ctrl Pts',(6.69345108162377,9.49192378686253,-3.75));
#7672=CARTESIAN_POINT('Ctrl Pts',(6.69345108162377,9.49192378686253,12.75));
#7673=CARTESIAN_POINT('Ctrl Pts',(6.68381150859182,9.55786385494286,-3.75));
#7674=CARTESIAN_POINT('Ctrl Pts',(6.68381150859182,9.55786385494286,12.75));
#7675=CARTESIAN_POINT('Ctrl Pts',(6.67359647366961,9.62389802250188,-3.75));
#7676=CARTESIAN_POINT('Ctrl Pts',(6.67359647366961,9.62389802250188,12.75));
#7677=CARTESIAN_POINT('Ctrl Pts',(6.66280711160719,9.69002090483258,-3.75));
#7678=CARTESIAN_POINT('Ctrl Pts',(6.66280711160719,9.69002090483258,12.75));
#7679=CARTESIAN_POINT('Ctrl Pts',(6.65144464725859,9.75622826411013,-3.75));
#7680=CARTESIAN_POINT('Ctrl Pts',(6.65144464725859,9.75622826411013,12.75));
#7681=CARTESIAN_POINT('Ctrl Pts',(6.63951038900667,9.82251725114898,-3.75));
#7682=CARTESIAN_POINT('Ctrl Pts',(6.63951038900667,9.82251725114898,12.75));
#7683=CARTESIAN_POINT('Ctrl Pts',(6.62700557693596,9.88888607996273,-3.75));
#7684=CARTESIAN_POINT('Ctrl Pts',(6.62700557693596,9.88888607996273,12.75));
#7685=CARTESIAN_POINT('Ctrl Pts',(6.61654612354183,9.94204425953052,-3.75));
#7686=CARTESIAN_POINT('Ctrl Pts',(6.61654612354183,9.94204425953052,12.75));
#7687=CARTESIAN_POINT('Ctrl Pts',(6.60844558393656,9.98194823089968,-3.75));
#7688=CARTESIAN_POINT('Ctrl Pts',(6.60844558393656,9.98194823089968,12.75));
#7689=CARTESIAN_POINT('Ctrl Pts',(6.60293150665659,10.0085665785717,-3.75));
#7690=CARTESIAN_POINT('Ctrl Pts',(6.60293150665659,10.0085665785717,12.75));
#7691=CARTESIAN_POINT('Ctrl Pts',(6.60014603862877,10.0218796774244,-3.75));
#7692=CARTESIAN_POINT('Ctrl Pts',(6.60014603862877,10.0218796774244,12.75));
#7693=CARTESIAN_POINT('Ctrl Pts',(6.06863042059311,5.89037560471066,-1.));
#7694=CARTESIAN_POINT('Ctrl Pts',(6.07642118935899,5.89793753402584,-1.));
#7695=CARTESIAN_POINT('Ctrl Pts',(6.09164867072823,5.91336588048663,-1.));
#7696=CARTESIAN_POINT('Ctrl Pts',(6.11342775487885,5.93742183851679,-1.));
#7697=CARTESIAN_POINT('Ctrl Pts',(6.14045331140034,5.97123031969246,-1.));
#7698=CARTESIAN_POINT('Ctrl Pts',(6.17151878498999,6.01584411654484,-1.));
#7699=CARTESIAN_POINT('Ctrl Pts',(6.20066685685755,6.06213722636286,-1.));
#7700=CARTESIAN_POINT('Ctrl Pts',(6.22866991793492,6.10945353793713,-1.));
#7701=CARTESIAN_POINT('Ctrl Pts',(6.25605474467853,6.15733614814835,-1.));
#7702=CARTESIAN_POINT('Ctrl Pts',(6.28297985424308,6.20562962932065,-1.));
#7703=CARTESIAN_POINT('Ctrl Pts',(6.30937750420801,6.2543646376197,-1.));
#7704=CARTESIAN_POINT('Ctrl Pts',(6.33505137069502,6.30367904881887,-1.));
#7705=CARTESIAN_POINT('Ctrl Pts',(6.35978286360965,6.35373180396277,-1.));
#7706=CARTESIAN_POINT('Ctrl Pts',(6.38345478017076,6.40460296268299,-1.));
#7707=CARTESIAN_POINT('Ctrl Pts',(6.40608444337878,6.45626649182452,-1.));
#7708=CARTESIAN_POINT('Ctrl Pts',(6.42776254872513,6.50863892931076,-1.));
#7709=CARTESIAN_POINT('Ctrl Pts',(6.44861636238489,6.56160843323028,-1.));
#7710=CARTESIAN_POINT('Ctrl Pts',(6.46876645798849,6.6150690793574,-1.));
#7711=CARTESIAN_POINT('Ctrl Pts',(6.48827758470623,6.66895976394944,-1.));
#7712=CARTESIAN_POINT('Ctrl Pts',(6.50715912032692,6.72326378902151,-1.));
#7713=CARTESIAN_POINT('Ctrl Pts',(6.52538888693356,6.77798990345396,-1.));
#7714=CARTESIAN_POINT('Ctrl Pts',(6.54292981913304,6.83315901897031,-1.));
#7715=CARTESIAN_POINT('Ctrl Pts',(6.5597485722992,6.88878938806037,-1.));
#7716=CARTESIAN_POINT('Ctrl Pts',(6.5758359541656,6.94488033148853,-1.));
#7717=CARTESIAN_POINT('Ctrl Pts',(6.5912030640433,7.00141528186886,-1.));
#7718=CARTESIAN_POINT('Ctrl Pts',(6.60587239994885,7.05836882883084,-1.));
#7719=CARTESIAN_POINT('Ctrl Pts',(6.61987066605911,7.11571241317029,-1.));
#7720=CARTESIAN_POINT('Ctrl Pts',(6.63322107969569,7.17342042004755,-1.));
#7721=CARTESIAN_POINT('Ctrl Pts',(6.64593535561053,7.23147652896403,-1.));
#7722=CARTESIAN_POINT('Ctrl Pts',(6.65801638970246,7.28987157005223,-1.));
#7723=CARTESIAN_POINT('Ctrl Pts',(6.66946176275797,7.34860073021491,-1.));
#7724=CARTESIAN_POINT('Ctrl Pts',(6.68026694677668,7.40766099640557,-1.));
#7725=CARTESIAN_POINT('Ctrl Pts',(6.69042862091104,7.46704851290034,-1.));
#7726=CARTESIAN_POINT('Ctrl Pts',(6.69994799095524,7.52675593674632,-1.));
#7727=CARTESIAN_POINT('Ctrl Pts',(6.70882947565318,7.58677347699226,-1.));
#7728=CARTESIAN_POINT('Ctrl Pts',(6.71707933277187,7.64708998288989,-1.));
#7729=CARTESIAN_POINT('Ctrl Pts',(6.72470431659336,7.70769400824503,-1.));
#7730=CARTESIAN_POINT('Ctrl Pts',(6.73171032576036,7.76857488460783,-1.));
#7731=CARTESIAN_POINT('Ctrl Pts',(6.73810106562749,7.82972378407324,-1.));
#7732=CARTESIAN_POINT('Ctrl Pts',(6.74387863902608,7.89113323756912,-1.));
#7733=CARTESIAN_POINT('Ctrl Pts',(6.7490441308376,7.95279665937614,-1.));
#7734=CARTESIAN_POINT('Ctrl Pts',(6.75359819949754,8.01470786732018,-1.));
#7735=CARTESIAN_POINT('Ctrl Pts',(6.75754166486089,8.07686060726827,-1.));
#7736=CARTESIAN_POINT('Ctrl Pts',(6.76087611417306,8.13924806419107,-1.));
#7737=CARTESIAN_POINT('Ctrl Pts',(6.7636036696164,8.20186305794855,-1.));
#7738=CARTESIAN_POINT('Ctrl Pts',(6.76572674650935,8.26469824786602,-1.));
#7739=CARTESIAN_POINT('Ctrl Pts',(6.76724781676282,8.32774633509908,-1.));
#7740=CARTESIAN_POINT('Ctrl Pts',(6.76816918165128,8.39100025749018,-1.));
#7741=CARTESIAN_POINT('Ctrl Pts',(6.76849272647565,8.45445340444926,-1.));
#7742=CARTESIAN_POINT('Ctrl Pts',(6.76822000004555,8.51809951610774,-1.));
#7743=CARTESIAN_POINT('Ctrl Pts',(6.76735232235635,8.58193255779939,-1.));
#7744=CARTESIAN_POINT('Ctrl Pts',(6.76589088878265,8.64594659806298,-1.));
#7745=CARTESIAN_POINT('Ctrl Pts',(6.76383687353853,8.71013569385599,-1.));
#7746=CARTESIAN_POINT('Ctrl Pts',(6.76119155448275,8.77449374557664,-1.));
#7747=CARTESIAN_POINT('Ctrl Pts',(6.7579562951925,8.83901457377471,-1.));
#7748=CARTESIAN_POINT('Ctrl Pts',(6.75413249860576,8.90369203916218,-1.));
#7749=CARTESIAN_POINT('Ctrl Pts',(6.74972157399229,8.96852015431046,-1.));
#7750=CARTESIAN_POINT('Ctrl Pts',(6.74472490424422,9.03349318036198,-1.));
#7751=CARTESIAN_POINT('Ctrl Pts',(6.73914381348523,9.09860577342165,-1.));
#7752=CARTESIAN_POINT('Ctrl Pts',(6.73297955932548,9.16385288053588,-1.));
#7753=CARTESIAN_POINT('Ctrl Pts',(6.72623333926846,9.22922952332026,-1.));
#7754=CARTESIAN_POINT('Ctrl Pts',(6.71890629646187,9.2947306015555,-1.));
#7755=CARTESIAN_POINT('Ctrl Pts',(6.71099953007124,9.36035072031876,-1.));
#7756=CARTESIAN_POINT('Ctrl Pts',(6.70251410760819,9.42608392519666,-1.));
#7757=CARTESIAN_POINT('Ctrl Pts',(6.69345108162377,9.49192378686253,-1.));
#7758=CARTESIAN_POINT('Ctrl Pts',(6.68381150859182,9.55786385494286,-1.));
#7759=CARTESIAN_POINT('Ctrl Pts',(6.67359647366961,9.62389802250188,-1.));
#7760=CARTESIAN_POINT('Ctrl Pts',(6.66280711160719,9.69002090483258,-1.));
#7761=CARTESIAN_POINT('Ctrl Pts',(6.65144464725859,9.75622826411013,-1.));
#7762=CARTESIAN_POINT('Ctrl Pts',(6.63951038900667,9.82251725114898,-1.));
#7763=CARTESIAN_POINT('Ctrl Pts',(6.62700557693596,9.88888607996273,-1.));
#7764=CARTESIAN_POINT('Ctrl Pts',(6.61654612354183,9.94204425953052,-1.));
#7765=CARTESIAN_POINT('Ctrl Pts',(6.60844558393656,9.98194823089968,-1.));
#7766=CARTESIAN_POINT('Ctrl Pts',(6.60293150665659,10.0085665785717,-1.));
#7767=CARTESIAN_POINT('Ctrl Pts',(6.60014603862877,10.0218796774244,-1.));
#7768=CARTESIAN_POINT('Ctrl Pts',(6.06863042059311,5.89037560471066,6.));
#7769=CARTESIAN_POINT('Ctrl Pts',(6.07642118935899,5.89793753402584,6.));
#7770=CARTESIAN_POINT('Ctrl Pts',(6.09164867072823,5.91336588048663,6.));
#7771=CARTESIAN_POINT('Ctrl Pts',(6.11342775487885,5.93742183851679,6.));
#7772=CARTESIAN_POINT('Ctrl Pts',(6.14045331140034,5.97123031969246,6.));
#7773=CARTESIAN_POINT('Ctrl Pts',(6.17151878498999,6.01584411654484,6.));
#7774=CARTESIAN_POINT('Ctrl Pts',(6.20066685685755,6.06213722636286,6.));
#7775=CARTESIAN_POINT('Ctrl Pts',(6.22866991793492,6.10945353793713,6.));
#7776=CARTESIAN_POINT('Ctrl Pts',(6.25605474467853,6.15733614814835,6.));
#7777=CARTESIAN_POINT('Ctrl Pts',(6.28297985424308,6.20562962932065,6.));
#7778=CARTESIAN_POINT('Ctrl Pts',(6.30937750420801,6.2543646376197,6.));
#7779=CARTESIAN_POINT('Ctrl Pts',(6.33505137069502,6.30367904881887,6.));
#7780=CARTESIAN_POINT('Ctrl Pts',(6.35978286360965,6.35373180396277,6.));
#7781=CARTESIAN_POINT('Ctrl Pts',(6.38345478017076,6.40460296268299,6.));
#7782=CARTESIAN_POINT('Ctrl Pts',(6.40608444337878,6.45626649182452,6.));
#7783=CARTESIAN_POINT('Ctrl Pts',(6.42776254872513,6.50863892931076,6.));
#7784=CARTESIAN_POINT('Ctrl Pts',(6.44861636238489,6.56160843323028,6.));
#7785=CARTESIAN_POINT('Ctrl Pts',(6.46876645798849,6.6150690793574,6.));
#7786=CARTESIAN_POINT('Ctrl Pts',(6.48827758470623,6.66895976394944,6.));
#7787=CARTESIAN_POINT('Ctrl Pts',(6.50715912032692,6.72326378902151,6.));
#7788=CARTESIAN_POINT('Ctrl Pts',(6.52538888693356,6.77798990345396,6.));
#7789=CARTESIAN_POINT('Ctrl Pts',(6.54292981913304,6.83315901897031,6.));
#7790=CARTESIAN_POINT('Ctrl Pts',(6.5597485722992,6.88878938806037,6.));
#7791=CARTESIAN_POINT('Ctrl Pts',(6.5758359541656,6.94488033148853,6.));
#7792=CARTESIAN_POINT('Ctrl Pts',(6.5912030640433,7.00141528186886,6.));
#7793=CARTESIAN_POINT('Ctrl Pts',(6.60587239994885,7.05836882883084,6.));
#7794=CARTESIAN_POINT('Ctrl Pts',(6.61987066605911,7.11571241317029,6.));
#7795=CARTESIAN_POINT('Ctrl Pts',(6.63322107969569,7.17342042004755,6.));
#7796=CARTESIAN_POINT('Ctrl Pts',(6.64593535561053,7.23147652896403,6.));
#7797=CARTESIAN_POINT('Ctrl Pts',(6.65801638970246,7.28987157005223,6.));
#7798=CARTESIAN_POINT('Ctrl Pts',(6.66946176275797,7.34860073021491,6.));
#7799=CARTESIAN_POINT('Ctrl Pts',(6.68026694677668,7.40766099640557,6.));
#7800=CARTESIAN_POINT('Ctrl Pts',(6.69042862091104,7.46704851290034,6.));
#7801=CARTESIAN_POINT('Ctrl Pts',(6.69994799095524,7.52675593674632,6.));
#7802=CARTESIAN_POINT('Ctrl Pts',(6.70882947565318,7.58677347699226,6.));
#7803=CARTESIAN_POINT('Ctrl Pts',(6.71707933277187,7.64708998288989,6.));
#7804=CARTESIAN_POINT('Ctrl Pts',(6.72470431659336,7.70769400824503,6.));
#7805=CARTESIAN_POINT('Ctrl Pts',(6.73171032576036,7.76857488460783,6.));
#7806=CARTESIAN_POINT('Ctrl Pts',(6.73810106562749,7.82972378407324,6.));
#7807=CARTESIAN_POINT('Ctrl Pts',(6.74387863902608,7.89113323756912,6.));
#7808=CARTESIAN_POINT('Ctrl Pts',(6.7490441308376,7.95279665937614,6.));
#7809=CARTESIAN_POINT('Ctrl Pts',(6.75359819949754,8.01470786732018,6.));
#7810=CARTESIAN_POINT('Ctrl Pts',(6.75754166486089,8.07686060726827,6.));
#7811=CARTESIAN_POINT('Ctrl Pts',(6.76087611417306,8.13924806419107,6.));
#7812=CARTESIAN_POINT('Ctrl Pts',(6.7636036696164,8.20186305794855,6.));
#7813=CARTESIAN_POINT('Ctrl Pts',(6.76572674650935,8.26469824786602,6.));
#7814=CARTESIAN_POINT('Ctrl Pts',(6.76724781676282,8.32774633509908,6.));
#7815=CARTESIAN_POINT('Ctrl Pts',(6.76816918165128,8.39100025749018,6.));
#7816=CARTESIAN_POINT('Ctrl Pts',(6.76849272647565,8.45445340444926,6.));
#7817=CARTESIAN_POINT('Ctrl Pts',(6.76822000004555,8.51809951610774,6.));
#7818=CARTESIAN_POINT('Ctrl Pts',(6.76735232235635,8.58193255779939,6.));
#7819=CARTESIAN_POINT('Ctrl Pts',(6.76589088878265,8.64594659806298,6.));
#7820=CARTESIAN_POINT('Ctrl Pts',(6.76383687353853,8.71013569385599,6.));
#7821=CARTESIAN_POINT('Ctrl Pts',(6.76119155448275,8.77449374557664,6.));
#7822=CARTESIAN_POINT('Ctrl Pts',(6.7579562951925,8.83901457377471,6.));
#7823=CARTESIAN_POINT('Ctrl Pts',(6.75413249860576,8.90369203916218,6.));
#7824=CARTESIAN_POINT('Ctrl Pts',(6.74972157399229,8.96852015431046,6.));
#7825=CARTESIAN_POINT('Ctrl Pts',(6.74472490424422,9.03349318036198,6.));
#7826=CARTESIAN_POINT('Ctrl Pts',(6.73914381348523,9.09860577342165,6.));
#7827=CARTESIAN_POINT('Ctrl Pts',(6.73297955932548,9.16385288053588,6.));
#7828=CARTESIAN_POINT('Ctrl Pts',(6.72623333926846,9.22922952332026,6.));
#7829=CARTESIAN_POINT('Ctrl Pts',(6.71890629646187,9.2947306015555,6.));
#7830=CARTESIAN_POINT('Ctrl Pts',(6.71099953007124,9.36035072031876,6.));
#7831=CARTESIAN_POINT('Ctrl Pts',(6.70251410760819,9.42608392519666,6.));
#7832=CARTESIAN_POINT('Ctrl Pts',(6.69345108162377,9.49192378686253,6.));
#7833=CARTESIAN_POINT('Ctrl Pts',(6.68381150859182,9.55786385494286,6.));
#7834=CARTESIAN_POINT('Ctrl Pts',(6.67359647366961,9.62389802250188,6.));
#7835=CARTESIAN_POINT('Ctrl Pts',(6.66280711160719,9.69002090483258,6.));
#7836=CARTESIAN_POINT('Ctrl Pts',(6.65144464725859,9.75622826411013,6.));
#7837=CARTESIAN_POINT('Ctrl Pts',(6.63951038900667,9.82251725114898,6.));
#7838=CARTESIAN_POINT('Ctrl Pts',(6.62700557693596,9.88888607996273,6.));
#7839=CARTESIAN_POINT('Ctrl Pts',(6.61654612354183,9.94204425953052,6.));
#7840=CARTESIAN_POINT('Ctrl Pts',(6.60844558393656,9.98194823089968,6.));
#7841=CARTESIAN_POINT('Ctrl Pts',(6.60293150665659,10.0085665785717,6.));
#7842=CARTESIAN_POINT('Ctrl Pts',(6.60014603862877,10.0218796774244,6.));
#7843=CARTESIAN_POINT('Origin',(0.,0.,-1.));
#7844=CARTESIAN_POINT('Origin',(0.,0.,-1.));
#7845=CARTESIAN_POINT('Origin',(0.,0.,-1.));
#7846=CARTESIAN_POINT('Origin',(0.,0.,-1.));
#7847=CARTESIAN_POINT('',(5.02458355455784,2.3072496837722,-1.));
#7848=CARTESIAN_POINT('Origin',(0.,0.,-1.));
#7849=CARTESIAN_POINT('',(6.20653880480254,1.76258817211517,-1.));
#7850=CARTESIAN_POINT('Origin',(5.93335250998519,2.72454931910811,-1.));
#7851=CARTESIAN_POINT('',(8.13553012180811,2.31040030805735,-1.));
#7852=CARTESIAN_POINT('',(4.06776506090406,1.15520015402867,-1.));
#7853=CARTESIAN_POINT('',(11.9792754136349,0.704954299427496,-1.));
#7854=CARTESIAN_POINT('Ctrl Pts',(11.9792754136349,0.704954299427529,-1.));
#7855=CARTESIAN_POINT('Ctrl Pts',(11.9691386658393,0.714023134927411,-1.));
#7856=CARTESIAN_POINT('Ctrl Pts',(11.9488435391885,0.73210763976631,-1.));
#7857=CARTESIAN_POINT('Ctrl Pts',(11.9183359560736,0.759074898533419,-1.));
#7858=CARTESIAN_POINT('Ctrl Pts',(11.877529348846,0.794712140666325,-1.));
#7859=CARTESIAN_POINT('Ctrl Pts',(11.8263046631092,0.838726039995982,-1.));
#7860=CARTESIAN_POINT('Ctrl Pts',(11.7748638454684,0.882205904336896,-1.));
#7861=CARTESIAN_POINT('Ctrl Pts',(11.7232078225909,0.925149766751161,-1.));
#7862=CARTESIAN_POINT('Ctrl Pts',(11.6713384077523,0.967555069553193,-1.));
#7863=CARTESIAN_POINT('Ctrl Pts',(11.6192586585895,1.00941863307588,-1.));
#7864=CARTESIAN_POINT('Ctrl Pts',(11.5669726710206,1.05073678224334,-1.));
#7865=CARTESIAN_POINT('Ctrl Pts',(11.5144851912285,1.09150552381395,-1.));
#7866=CARTESIAN_POINT('Ctrl Pts',(11.4618012771636,1.13172071766774,-1.));
#7867=CARTESIAN_POINT('Ctrl Pts',(11.4089259705106,1.17137823760545,-1.));
#7868=CARTESIAN_POINT('Ctrl Pts',(11.3558638941869,1.21047418192819,-1.));
#7869=CARTESIAN_POINT('Ctrl Pts',(11.30261917075,1.24900490126928,-1.));
#7870=CARTESIAN_POINT('Ctrl Pts',(11.2491956455455,1.28696685552412,-1.));
#7871=CARTESIAN_POINT('Ctrl Pts',(11.1955970312291,1.32435651843207,-1.));
#7872=CARTESIAN_POINT('Ctrl Pts',(11.1418270749817,1.36117027439398,-1.));
#7873=CARTESIAN_POINT('Ctrl Pts',(11.0878897426906,1.39740430473756,-1.));
#7874=CARTESIAN_POINT('Ctrl Pts',(11.033789312906,1.43305454241432,-1.));
#7875=CARTESIAN_POINT('Ctrl Pts',(10.9795302662584,1.46811677324654,-1.));
#7876=CARTESIAN_POINT('Ctrl Pts',(10.9251172180581,1.50258671261028,-1.));
#7877=CARTESIAN_POINT('Ctrl Pts',(10.8705548380775,1.53646008988796,-1.));
#7878=CARTESIAN_POINT('Ctrl Pts',(10.8158477697972,1.56973274862052,-1.));
#7879=CARTESIAN_POINT('Ctrl Pts',(10.761000572936,1.60240070038749,-1.));
#7880=CARTESIAN_POINT('Ctrl Pts',(10.7060177866027,1.63445994423348,-1.));
#7881=CARTESIAN_POINT('Ctrl Pts',(10.6509039769739,1.66590631967585,-1.));
#7882=CARTESIAN_POINT('Ctrl Pts',(10.59566379085,1.69673535547184,-1.));
#7883=CARTESIAN_POINT('Ctrl Pts',(10.5403020105194,1.72694211360792,-1.));
#7884=CARTESIAN_POINT('Ctrl Pts',(10.4848236013528,1.75652107004318,-1.));
#7885=CARTESIAN_POINT('Ctrl Pts',(10.4292336483793,1.78546643461776,-1.));
#7886=CARTESIAN_POINT('Ctrl Pts',(10.3735373011506,1.81377244526718,-1.));
#7887=CARTESIAN_POINT('Ctrl Pts',(10.317739716759,1.84143367405762,-1.));
#7888=CARTESIAN_POINT('Ctrl Pts',(10.2618460035706,1.86844533887956,-1.));
#7889=CARTESIAN_POINT('Ctrl Pts',(10.2058611678956,1.89480360265125,-1.));
#7890=CARTESIAN_POINT('Ctrl Pts',(10.1497902344364,1.92050480406378,-1.));
#7891=CARTESIAN_POINT('Ctrl Pts',(10.0936383641523,1.94554471072257,-1.));
#7892=CARTESIAN_POINT('Ctrl Pts',(10.037410974034,1.96991776698621,-1.));
#7893=CARTESIAN_POINT('Ctrl Pts',(9.98111385659409,1.99361634997092,-1.));
#7894=CARTESIAN_POINT('Ctrl Pts',(9.92475330165988,2.01663001707736,-1.));
#7895=CARTESIAN_POINT('Ctrl Pts',(9.86833584478527,2.03894719582859,-1.));
#7896=CARTESIAN_POINT('Ctrl Pts',(9.81186801391803,2.06055689146528,-1.));
#7897=CARTESIAN_POINT('Ctrl Pts',(9.75535607889871,2.08145038176732,-1.));
#7898=CARTESIAN_POINT('Ctrl Pts',(9.69880579601398,2.10162295100989,-1.));
#7899=CARTESIAN_POINT('Ctrl Pts',(9.64222216484242,2.12107554726937,-1.));
#7900=CARTESIAN_POINT('Ctrl Pts',(9.58561005875903,2.13981058538587,-1.));
#7901=CARTESIAN_POINT('Ctrl Pts',(9.52897485563506,2.15782775391113,-1.));
#7902=CARTESIAN_POINT('Ctrl Pts',(9.4723230488593,2.17511995998945,-1.));
#7903=CARTESIAN_POINT('Ctrl Pts',(9.41566291502215,2.19166889809876,-1.));
#7904=CARTESIAN_POINT('Ctrl Pts',(9.35900502856467,2.2074416540289,-1.));
#7905=CARTESIAN_POINT('Ctrl Pts',(9.30236077039477,2.22240082168223,-1.));
#7906=CARTESIAN_POINT('Ctrl Pts',(9.24574089753053,2.23651421201962,-1.));
#7907=CARTESIAN_POINT('Ctrl Pts',(9.18915420809356,2.24976392906278,-1.));
#7908=CARTESIAN_POINT('Ctrl Pts',(9.13260588645235,2.26215759393014,-1.));
#7909=CARTESIAN_POINT('Ctrl Pts',(9.07609679780011,2.27373321015996,-1.));
#7910=CARTESIAN_POINT('Ctrl Pts',(9.0196273647496,2.28453333318601,-1.));
#7911=CARTESIAN_POINT('Ctrl Pts',(8.96320109950669,2.29458154408801,-1.));
#7912=CARTESIAN_POINT('Ctrl Pts',(8.90682777405608,2.30386137247017,-1.));
#7913=CARTESIAN_POINT('Ctrl Pts',(8.85052793120604,2.31228619203479,-1.));
#7914=CARTESIAN_POINT('Ctrl Pts',(8.79433301721166,2.31969862084206,-1.));
#7915=CARTESIAN_POINT('Ctrl Pts',(8.73827625692193,2.32593252219559,-1.));
#7916=CARTESIAN_POINT('Ctrl Pts',(8.68238458286971,2.33086762045752,-1.));
#7917=CARTESIAN_POINT('Ctrl Pts',(8.62667187892838,2.33447589689188,-1.));
#7918=CARTESIAN_POINT('Ctrl Pts',(8.57112741281372,2.33689888190034,-1.));
#7919=CARTESIAN_POINT('Ctrl Pts',(8.51572283259063,2.33840535058003,-1.));
#7920=CARTESIAN_POINT('Ctrl Pts',(8.46043689627596,2.3392342622836,-1.));
#7921=CARTESIAN_POINT('Ctrl Pts',(8.40527692606173,2.339459611751,-1.));
#7922=CARTESIAN_POINT('Ctrl Pts',(8.35029826768635,2.33886640526141,-1.));
#7923=CARTESIAN_POINT('Ctrl Pts',(8.29563322262997,2.33676998946178,-1.));
#7924=CARTESIAN_POINT('Ctrl Pts',(8.24146380440172,2.33217339857873,-1.));
#7925=CARTESIAN_POINT('Ctrl Pts',(8.19867202257947,2.32567282066755,-1.));
#7926=CARTESIAN_POINT('Ctrl Pts',(8.16694940973767,2.31883955953704,-1.));
#7927=CARTESIAN_POINT('Ctrl Pts',(8.14597432907962,2.31336634706602,-1.));
#7928=CARTESIAN_POINT('Ctrl Pts',(8.13553012180811,2.31040030805735,-1.));
#7929=CARTESIAN_POINT('',(11.9792754136349,-0.704954299427528,-1.));
#7930=CARTESIAN_POINT('Origin',(3.99680288865056E-13,0.,-1.));
#7931=CARTESIAN_POINT('',(8.13553012180811,-2.31040030805735,-1.));
#7932=CARTESIAN_POINT('Ctrl Pts',(8.13553012180811,-2.31040030805735,-1.));
#7933=CARTESIAN_POINT('Ctrl Pts',(8.14597432907962,-2.31336634706602,-1.));
#7934=CARTESIAN_POINT('Ctrl Pts',(8.16694940973767,-2.31883955953704,-1.));
#7935=CARTESIAN_POINT('Ctrl Pts',(8.19867202257947,-2.32567282066755,-1.));
#7936=CARTESIAN_POINT('Ctrl Pts',(8.24146380440172,-2.33217339857873,-1.));
#7937=CARTESIAN_POINT('Ctrl Pts',(8.29563322262997,-2.33676998946178,-1.));
#7938=CARTESIAN_POINT('Ctrl Pts',(8.35029826768635,-2.33886640526141,-1.));
#7939=CARTESIAN_POINT('Ctrl Pts',(8.40527692606173,-2.339459611751,-1.));
#7940=CARTESIAN_POINT('Ctrl Pts',(8.46043689627596,-2.3392342622836,-1.));
#7941=CARTESIAN_POINT('Ctrl Pts',(8.51572283259063,-2.33840535058003,-1.));
#7942=CARTESIAN_POINT('Ctrl Pts',(8.57112741281372,-2.33689888190034,-1.));
#7943=CARTESIAN_POINT('Ctrl Pts',(8.62667187892838,-2.33447589689188,-1.));
#7944=CARTESIAN_POINT('Ctrl Pts',(8.68238458286971,-2.33086762045752,-1.));
#7945=CARTESIAN_POINT('Ctrl Pts',(8.73827625692193,-2.32593252219559,-1.));
#7946=CARTESIAN_POINT('Ctrl Pts',(8.79433301721166,-2.31969862084206,-1.));
#7947=CARTESIAN_POINT('Ctrl Pts',(8.85052793120604,-2.31228619203479,-1.));
#7948=CARTESIAN_POINT('Ctrl Pts',(8.90682777405608,-2.30386137247017,-1.));
#7949=CARTESIAN_POINT('Ctrl Pts',(8.96320109950669,-2.29458154408801,-1.));
#7950=CARTESIAN_POINT('Ctrl Pts',(9.0196273647496,-2.28453333318601,-1.));
#7951=CARTESIAN_POINT('Ctrl Pts',(9.07609679780011,-2.27373321015996,-1.));
#7952=CARTESIAN_POINT('Ctrl Pts',(9.13260588645235,-2.26215759393014,-1.));
#7953=CARTESIAN_POINT('Ctrl Pts',(9.18915420809356,-2.24976392906278,-1.));
#7954=CARTESIAN_POINT('Ctrl Pts',(9.24574089753053,-2.23651421201962,-1.));
#7955=CARTESIAN_POINT('Ctrl Pts',(9.30236077039477,-2.22240082168223,-1.));
#7956=CARTESIAN_POINT('Ctrl Pts',(9.35900502856467,-2.2074416540289,-1.));
#7957=CARTESIAN_POINT('Ctrl Pts',(9.41566291502215,-2.19166889809876,-1.));
#7958=CARTESIAN_POINT('Ctrl Pts',(9.4723230488593,-2.17511995998945,-1.));
#7959=CARTESIAN_POINT('Ctrl Pts',(9.52897485563506,-2.15782775391113,-1.));
#7960=CARTESIAN_POINT('Ctrl Pts',(9.58561005875903,-2.13981058538587,-1.));
#7961=CARTESIAN_POINT('Ctrl Pts',(9.64222216484242,-2.12107554726937,-1.));
#7962=CARTESIAN_POINT('Ctrl Pts',(9.69880579601398,-2.10162295100989,-1.));
#7963=CARTESIAN_POINT('Ctrl Pts',(9.75535607889871,-2.08145038176732,-1.));
#7964=CARTESIAN_POINT('Ctrl Pts',(9.81186801391803,-2.06055689146528,-1.));
#7965=CARTESIAN_POINT('Ctrl Pts',(9.86833584478527,-2.03894719582859,-1.));
#7966=CARTESIAN_POINT('Ctrl Pts',(9.92475330165988,-2.01663001707736,-1.));
#7967=CARTESIAN_POINT('Ctrl Pts',(9.98111385659409,-1.99361634997092,-1.));
#7968=CARTESIAN_POINT('Ctrl Pts',(10.037410974034,-1.96991776698621,-1.));
#7969=CARTESIAN_POINT('Ctrl Pts',(10.0936383641523,-1.94554471072257,-1.));
#7970=CARTESIAN_POINT('Ctrl Pts',(10.1497902344364,-1.92050480406378,-1.));
#7971=CARTESIAN_POINT('Ctrl Pts',(10.2058611678956,-1.89480360265125,-1.));
#7972=CARTESIAN_POINT('Ctrl Pts',(10.2618460035706,-1.86844533887956,-1.));
#7973=CARTESIAN_POINT('Ctrl Pts',(10.317739716759,-1.84143367405762,-1.));
#7974=CARTESIAN_POINT('Ctrl Pts',(10.3735373011506,-1.81377244526718,-1.));
#7975=CARTESIAN_POINT('Ctrl Pts',(10.4292336483793,-1.78546643461776,-1.));
#7976=CARTESIAN_POINT('Ctrl Pts',(10.4848236013528,-1.75652107004318,-1.));
#7977=CARTESIAN_POINT('Ctrl Pts',(10.5403020105194,-1.72694211360792,-1.));
#7978=CARTESIAN_POINT('Ctrl Pts',(10.59566379085,-1.69673535547184,-1.));
#7979=CARTESIAN_POINT('Ctrl Pts',(10.6509039769739,-1.66590631967585,-1.));
#7980=CARTESIAN_POINT('Ctrl Pts',(10.7060177866027,-1.63445994423348,-1.));
#7981=CARTESIAN_POINT('Ctrl Pts',(10.761000572936,-1.60240070038749,-1.));
#7982=CARTESIAN_POINT('Ctrl Pts',(10.8158477697972,-1.56973274862052,-1.));
#7983=CARTESIAN_POINT('Ctrl Pts',(10.8705548380775,-1.53646008988796,-1.));
#7984=CARTESIAN_POINT('Ctrl Pts',(10.9251172180581,-1.50258671261028,-1.));
#7985=CARTESIAN_POINT('Ctrl Pts',(10.9795302662584,-1.46811677324654,-1.));
#7986=CARTESIAN_POINT('Ctrl Pts',(11.033789312906,-1.43305454241432,-1.));
#7987=CARTESIAN_POINT('Ctrl Pts',(11.0878897426906,-1.39740430473756,-1.));
#7988=CARTESIAN_POINT('Ctrl Pts',(11.1418270749817,-1.36117027439398,-1.));
#7989=CARTESIAN_POINT('Ctrl Pts',(11.1955970312291,-1.32435651843207,-1.));
#7990=CARTESIAN_POINT('Ctrl Pts',(11.2491956455455,-1.28696685552412,-1.));
#7991=CARTESIAN_POINT('Ctrl Pts',(11.30261917075,-1.24900490126928,-1.));
#7992=CARTESIAN_POINT('Ctrl Pts',(11.3558638941869,-1.21047418192819,-1.));
#7993=CARTESIAN_POINT('Ctrl Pts',(11.4089259705106,-1.17137823760545,-1.));
#7994=CARTESIAN_POINT('Ctrl Pts',(11.4618012771636,-1.13172071766774,-1.));
#7995=CARTESIAN_POINT('Ctrl Pts',(11.5144851912285,-1.09150552381395,-1.));
#7996=CARTESIAN_POINT('Ctrl Pts',(11.5669726710206,-1.05073678224334,-1.));
#7997=CARTESIAN_POINT('Ctrl Pts',(11.6192586585895,-1.00941863307588,-1.));
#7998=CARTESIAN_POINT('Ctrl Pts',(11.6713384077523,-0.967555069553193,-1.));
#7999=CARTESIAN_POINT('Ctrl Pts',(11.7232078225909,-0.925149766751161,-1.));
#8000=CARTESIAN_POINT('Ctrl Pts',(11.7748638454684,-0.882205904336896,-1.));
#8001=CARTESIAN_POINT('Ctrl Pts',(11.8263046631092,-0.838726039995982,-1.));
#8002=CARTESIAN_POINT('Ctrl Pts',(11.877529348846,-0.794712140666325,-1.));
#8003=CARTESIAN_POINT('Ctrl Pts',(11.9183359560736,-0.759074898533419,-1.));
#8004=CARTESIAN_POINT('Ctrl Pts',(11.9488435391885,-0.73210763976631,-1.));
#8005=CARTESIAN_POINT('Ctrl Pts',(11.9691386658393,-0.714023134927411,-1.));
#8006=CARTESIAN_POINT('Ctrl Pts',(11.9792754136349,-0.704954299427529,-1.));
#8007=CARTESIAN_POINT('',(6.20653880480254,-1.76258817211517,-1.));
#8008=CARTESIAN_POINT('',(2.65453178512701,-0.75385758054847,-1.));
#8009=CARTESIAN_POINT('',(5.02458355455784,-2.3072496837722,-1.));
#8010=CARTESIAN_POINT('Origin',(5.93335250998519,-2.72454931910811,-1.));
#8011=CARTESIAN_POINT('Origin',(0.,0.,-1.));
#8012=CARTESIAN_POINT('Origin',(0.,0.,-1.));
#8013=CARTESIAN_POINT('',(-5.,6.12323399573677E-16,-1.));
#8014=CARTESIAN_POINT('Origin',(0.,0.,-1.));
#8015=CARTESIAN_POINT('Origin',(0.,0.,0.));
#8016=CARTESIAN_POINT('',(5.02458355455784,2.3072496837722,6.));
#8017=CARTESIAN_POINT('Origin',(0.,0.,6.));
#8018=CARTESIAN_POINT('',(5.02458355455784,2.3072496837722,0.));
#8019=CARTESIAN_POINT('Origin',(0.,0.,0.));
#8020=CARTESIAN_POINT('Origin',(0.,0.,6.));
#8021=CARTESIAN_POINT('Origin',(0.,0.,0.));
#8022=CARTESIAN_POINT('Origin',(0.,0.,6.));
#8023=CARTESIAN_POINT('Origin',(0.,0.,0.));
#8024=CARTESIAN_POINT('Origin',(0.,0.,6.));
#8025=CARTESIAN_POINT('Origin',(0.,0.,0.));
#8026=CARTESIAN_POINT('Origin',(0.,0.,6.));
#8027=CARTESIAN_POINT('Origin',(5.93335250998519,2.72454931910811,0.));
#8028=CARTESIAN_POINT('',(6.20653880480254,1.76258817211517,6.));
#8029=CARTESIAN_POINT('Origin',(5.93335250998519,2.72454931910811,6.));
#8030=CARTESIAN_POINT('',(6.20653880480254,1.76258817211517,0.));
#8031=CARTESIAN_POINT('Origin',(8.13553012180811,2.31040030805735,0.));
#8032=CARTESIAN_POINT('',(8.13553012180811,2.31040030805735,6.));
#8033=CARTESIAN_POINT('',(4.06776506090406,1.15520015402867,6.));
#8034=CARTESIAN_POINT('',(8.13553012180811,2.31040030805735,0.));
#8035=CARTESIAN_POINT('Origin',(5.93335250998519,-2.72454931910811,0.));
#8036=CARTESIAN_POINT('',(6.20653880480254,-1.76258817211517,6.));
#8037=CARTESIAN_POINT('',(6.20653880480254,-1.76258817211517,0.));
#8038=CARTESIAN_POINT('',(5.02458355455784,-2.3072496837722,6.));
#8039=CARTESIAN_POINT('Origin',(5.93335250998519,-2.72454931910811,6.));
#8040=CARTESIAN_POINT('',(5.02458355455784,-2.3072496837722,0.));
#8041=CARTESIAN_POINT('Origin',(5.30906357025403,-1.50771516109694,0.));
#8042=CARTESIAN_POINT('',(8.13553012180811,-2.31040030805735,6.));
#8043=CARTESIAN_POINT('',(8.13553012180811,-2.31040030805735,0.));
#8044=CARTESIAN_POINT('',(2.65453178512701,-0.75385758054847,6.));
#8045=CARTESIAN_POINT('Ctrl Pts',(11.9792754136349,0.704954299427529,-3.75));
#8046=CARTESIAN_POINT('Ctrl Pts',(11.9792754136349,0.704954299427529,12.75));
#8047=CARTESIAN_POINT('Ctrl Pts',(11.9691386658393,0.714023134927411,-3.75));
#8048=CARTESIAN_POINT('Ctrl Pts',(11.9691386658393,0.714023134927411,12.75));
#8049=CARTESIAN_POINT('Ctrl Pts',(11.9488435391885,0.73210763976631,-3.75));
#8050=CARTESIAN_POINT('Ctrl Pts',(11.9488435391885,0.73210763976631,12.75));
#8051=CARTESIAN_POINT('Ctrl Pts',(11.9183359560736,0.759074898533419,-3.75));
#8052=CARTESIAN_POINT('Ctrl Pts',(11.9183359560736,0.759074898533419,12.75));
#8053=CARTESIAN_POINT('Ctrl Pts',(11.877529348846,0.794712140666325,-3.75));
#8054=CARTESIAN_POINT('Ctrl Pts',(11.877529348846,0.794712140666325,12.75));
#8055=CARTESIAN_POINT('Ctrl Pts',(11.8263046631092,0.838726039995982,-3.75));
#8056=CARTESIAN_POINT('Ctrl Pts',(11.8263046631092,0.838726039995982,12.75));
#8057=CARTESIAN_POINT('Ctrl Pts',(11.7748638454684,0.882205904336896,-3.75));
#8058=CARTESIAN_POINT('Ctrl Pts',(11.7748638454684,0.882205904336896,12.75));
#8059=CARTESIAN_POINT('Ctrl Pts',(11.7232078225909,0.925149766751161,-3.75));
#8060=CARTESIAN_POINT('Ctrl Pts',(11.7232078225909,0.925149766751161,12.75));
#8061=CARTESIAN_POINT('Ctrl Pts',(11.6713384077523,0.967555069553193,-3.75));
#8062=CARTESIAN_POINT('Ctrl Pts',(11.6713384077523,0.967555069553193,12.75));
#8063=CARTESIAN_POINT('Ctrl Pts',(11.6192586585895,1.00941863307588,-3.75));
#8064=CARTESIAN_POINT('Ctrl Pts',(11.6192586585895,1.00941863307588,12.75));
#8065=CARTESIAN_POINT('Ctrl Pts',(11.5669726710206,1.05073678224334,-3.75));
#8066=CARTESIAN_POINT('Ctrl Pts',(11.5669726710206,1.05073678224334,12.75));
#8067=CARTESIAN_POINT('Ctrl Pts',(11.5144851912285,1.09150552381395,-3.75));
#8068=CARTESIAN_POINT('Ctrl Pts',(11.5144851912285,1.09150552381395,12.75));
#8069=CARTESIAN_POINT('Ctrl Pts',(11.4618012771636,1.13172071766774,-3.75));
#8070=CARTESIAN_POINT('Ctrl Pts',(11.4618012771636,1.13172071766774,12.75));
#8071=CARTESIAN_POINT('Ctrl Pts',(11.4089259705106,1.17137823760545,-3.75));
#8072=CARTESIAN_POINT('Ctrl Pts',(11.4089259705106,1.17137823760545,12.75));
#8073=CARTESIAN_POINT('Ctrl Pts',(11.3558638941869,1.21047418192819,-3.75));
#8074=CARTESIAN_POINT('Ctrl Pts',(11.3558638941869,1.21047418192819,12.75));
#8075=CARTESIAN_POINT('Ctrl Pts',(11.30261917075,1.24900490126928,-3.75));
#8076=CARTESIAN_POINT('Ctrl Pts',(11.30261917075,1.24900490126928,12.75));
#8077=CARTESIAN_POINT('Ctrl Pts',(11.2491956455455,1.28696685552412,-3.75));
#8078=CARTESIAN_POINT('Ctrl Pts',(11.2491956455455,1.28696685552412,12.75));
#8079=CARTESIAN_POINT('Ctrl Pts',(11.1955970312291,1.32435651843207,-3.75));
#8080=CARTESIAN_POINT('Ctrl Pts',(11.1955970312291,1.32435651843207,12.75));
#8081=CARTESIAN_POINT('Ctrl Pts',(11.1418270749817,1.36117027439398,-3.75));
#8082=CARTESIAN_POINT('Ctrl Pts',(11.1418270749817,1.36117027439398,12.75));
#8083=CARTESIAN_POINT('Ctrl Pts',(11.0878897426906,1.39740430473756,-3.75));
#8084=CARTESIAN_POINT('Ctrl Pts',(11.0878897426906,1.39740430473756,12.75));
#8085=CARTESIAN_POINT('Ctrl Pts',(11.033789312906,1.43305454241432,-3.75));
#8086=CARTESIAN_POINT('Ctrl Pts',(11.033789312906,1.43305454241432,12.75));
#8087=CARTESIAN_POINT('Ctrl Pts',(10.9795302662584,1.46811677324654,-3.75));
#8088=CARTESIAN_POINT('Ctrl Pts',(10.9795302662584,1.46811677324654,12.75));
#8089=CARTESIAN_POINT('Ctrl Pts',(10.9251172180581,1.50258671261028,-3.75));
#8090=CARTESIAN_POINT('Ctrl Pts',(10.9251172180581,1.50258671261028,12.75));
#8091=CARTESIAN_POINT('Ctrl Pts',(10.8705548380775,1.53646008988796,-3.75));
#8092=CARTESIAN_POINT('Ctrl Pts',(10.8705548380775,1.53646008988796,12.75));
#8093=CARTESIAN_POINT('Ctrl Pts',(10.8158477697972,1.56973274862052,-3.75));
#8094=CARTESIAN_POINT('Ctrl Pts',(10.8158477697972,1.56973274862052,12.75));
#8095=CARTESIAN_POINT('Ctrl Pts',(10.761000572936,1.60240070038749,-3.75));
#8096=CARTESIAN_POINT('Ctrl Pts',(10.761000572936,1.60240070038749,12.75));
#8097=CARTESIAN_POINT('Ctrl Pts',(10.7060177866027,1.63445994423348,-3.75));
#8098=CARTESIAN_POINT('Ctrl Pts',(10.7060177866027,1.63445994423348,12.75));
#8099=CARTESIAN_POINT('Ctrl Pts',(10.6509039769739,1.66590631967585,-3.75));
#8100=CARTESIAN_POINT('Ctrl Pts',(10.6509039769739,1.66590631967585,12.75));
#8101=CARTESIAN_POINT('Ctrl Pts',(10.59566379085,1.69673535547184,-3.75));
#8102=CARTESIAN_POINT('Ctrl Pts',(10.59566379085,1.69673535547184,12.75));
#8103=CARTESIAN_POINT('Ctrl Pts',(10.5403020105194,1.72694211360792,-3.75));
#8104=CARTESIAN_POINT('Ctrl Pts',(10.5403020105194,1.72694211360792,12.75));
#8105=CARTESIAN_POINT('Ctrl Pts',(10.4848236013528,1.75652107004318,-3.75));
#8106=CARTESIAN_POINT('Ctrl Pts',(10.4848236013528,1.75652107004318,12.75));
#8107=CARTESIAN_POINT('Ctrl Pts',(10.4292336483793,1.78546643461776,-3.75));
#8108=CARTESIAN_POINT('Ctrl Pts',(10.4292336483793,1.78546643461776,12.75));
#8109=CARTESIAN_POINT('Ctrl Pts',(10.3735373011506,1.81377244526718,-3.75));
#8110=CARTESIAN_POINT('Ctrl Pts',(10.3735373011506,1.81377244526718,12.75));
#8111=CARTESIAN_POINT('Ctrl Pts',(10.317739716759,1.84143367405762,-3.75));
#8112=CARTESIAN_POINT('Ctrl Pts',(10.317739716759,1.84143367405762,12.75));
#8113=CARTESIAN_POINT('Ctrl Pts',(10.2618460035706,1.86844533887956,-3.75));
#8114=CARTESIAN_POINT('Ctrl Pts',(10.2618460035706,1.86844533887956,12.75));
#8115=CARTESIAN_POINT('Ctrl Pts',(10.2058611678956,1.89480360265125,-3.75));
#8116=CARTESIAN_POINT('Ctrl Pts',(10.2058611678956,1.89480360265125,12.75));
#8117=CARTESIAN_POINT('Ctrl Pts',(10.1497902344364,1.92050480406378,-3.75));
#8118=CARTESIAN_POINT('Ctrl Pts',(10.1497902344364,1.92050480406378,12.75));
#8119=CARTESIAN_POINT('Ctrl Pts',(10.0936383641523,1.94554471072257,-3.75));
#8120=CARTESIAN_POINT('Ctrl Pts',(10.0936383641523,1.94554471072257,12.75));
#8121=CARTESIAN_POINT('Ctrl Pts',(10.037410974034,1.96991776698621,-3.75));
#8122=CARTESIAN_POINT('Ctrl Pts',(10.037410974034,1.96991776698621,12.75));
#8123=CARTESIAN_POINT('Ctrl Pts',(9.98111385659409,1.99361634997092,-3.75));
#8124=CARTESIAN_POINT('Ctrl Pts',(9.98111385659409,1.99361634997092,12.75));
#8125=CARTESIAN_POINT('Ctrl Pts',(9.92475330165988,2.01663001707736,-3.75));
#8126=CARTESIAN_POINT('Ctrl Pts',(9.92475330165988,2.01663001707736,12.75));
#8127=CARTESIAN_POINT('Ctrl Pts',(9.86833584478527,2.03894719582859,-3.75));
#8128=CARTESIAN_POINT('Ctrl Pts',(9.86833584478527,2.03894719582859,12.75));
#8129=CARTESIAN_POINT('Ctrl Pts',(9.81186801391803,2.06055689146528,-3.75));
#8130=CARTESIAN_POINT('Ctrl Pts',(9.81186801391803,2.06055689146528,12.75));
#8131=CARTESIAN_POINT('Ctrl Pts',(9.75535607889871,2.08145038176732,-3.75));
#8132=CARTESIAN_POINT('Ctrl Pts',(9.75535607889871,2.08145038176732,12.75));
#8133=CARTESIAN_POINT('Ctrl Pts',(9.69880579601398,2.10162295100989,-3.75));
#8134=CARTESIAN_POINT('Ctrl Pts',(9.69880579601398,2.10162295100989,12.75));
#8135=CARTESIAN_POINT('Ctrl Pts',(9.64222216484242,2.12107554726937,-3.75));
#8136=CARTESIAN_POINT('Ctrl Pts',(9.64222216484242,2.12107554726937,12.75));
#8137=CARTESIAN_POINT('Ctrl Pts',(9.58561005875903,2.13981058538587,-3.75));
#8138=CARTESIAN_POINT('Ctrl Pts',(9.58561005875903,2.13981058538587,12.75));
#8139=CARTESIAN_POINT('Ctrl Pts',(9.52897485563506,2.15782775391113,-3.75));
#8140=CARTESIAN_POINT('Ctrl Pts',(9.52897485563506,2.15782775391113,12.75));
#8141=CARTESIAN_POINT('Ctrl Pts',(9.4723230488593,2.17511995998945,-3.75));
#8142=CARTESIAN_POINT('Ctrl Pts',(9.4723230488593,2.17511995998945,12.75));
#8143=CARTESIAN_POINT('Ctrl Pts',(9.41566291502215,2.19166889809876,-3.75));
#8144=CARTESIAN_POINT('Ctrl Pts',(9.41566291502215,2.19166889809876,12.75));
#8145=CARTESIAN_POINT('Ctrl Pts',(9.35900502856467,2.2074416540289,-3.75));
#8146=CARTESIAN_POINT('Ctrl Pts',(9.35900502856467,2.2074416540289,12.75));
#8147=CARTESIAN_POINT('Ctrl Pts',(9.30236077039477,2.22240082168223,-3.75));
#8148=CARTESIAN_POINT('Ctrl Pts',(9.30236077039477,2.22240082168223,12.75));
#8149=CARTESIAN_POINT('Ctrl Pts',(9.24574089753053,2.23651421201962,-3.75));
#8150=CARTESIAN_POINT('Ctrl Pts',(9.24574089753053,2.23651421201962,12.75));
#8151=CARTESIAN_POINT('Ctrl Pts',(9.18915420809356,2.24976392906278,-3.75));
#8152=CARTESIAN_POINT('Ctrl Pts',(9.18915420809356,2.24976392906278,12.75));
#8153=CARTESIAN_POINT('Ctrl Pts',(9.13260588645235,2.26215759393014,-3.75));
#8154=CARTESIAN_POINT('Ctrl Pts',(9.13260588645235,2.26215759393014,12.75));
#8155=CARTESIAN_POINT('Ctrl Pts',(9.07609679780011,2.27373321015996,-3.75));
#8156=CARTESIAN_POINT('Ctrl Pts',(9.07609679780011,2.27373321015996,12.75));
#8157=CARTESIAN_POINT('Ctrl Pts',(9.0196273647496,2.28453333318601,-3.75));
#8158=CARTESIAN_POINT('Ctrl Pts',(9.0196273647496,2.28453333318601,12.75));
#8159=CARTESIAN_POINT('Ctrl Pts',(8.96320109950669,2.29458154408801,-3.75));
#8160=CARTESIAN_POINT('Ctrl Pts',(8.96320109950669,2.29458154408801,12.75));
#8161=CARTESIAN_POINT('Ctrl Pts',(8.90682777405608,2.30386137247017,-3.75));
#8162=CARTESIAN_POINT('Ctrl Pts',(8.90682777405608,2.30386137247017,12.75));
#8163=CARTESIAN_POINT('Ctrl Pts',(8.85052793120604,2.31228619203479,-3.75));
#8164=CARTESIAN_POINT('Ctrl Pts',(8.85052793120604,2.31228619203479,12.75));
#8165=CARTESIAN_POINT('Ctrl Pts',(8.79433301721166,2.31969862084206,-3.75));
#8166=CARTESIAN_POINT('Ctrl Pts',(8.79433301721166,2.31969862084206,12.75));
#8167=CARTESIAN_POINT('Ctrl Pts',(8.73827625692193,2.32593252219559,-3.75));
#8168=CARTESIAN_POINT('Ctrl Pts',(8.73827625692193,2.32593252219559,12.75));
#8169=CARTESIAN_POINT('Ctrl Pts',(8.68238458286971,2.33086762045752,-3.75));
#8170=CARTESIAN_POINT('Ctrl Pts',(8.68238458286971,2.33086762045752,12.75));
#8171=CARTESIAN_POINT('Ctrl Pts',(8.62667187892838,2.33447589689188,-3.75));
#8172=CARTESIAN_POINT('Ctrl Pts',(8.62667187892838,2.33447589689188,12.75));
#8173=CARTESIAN_POINT('Ctrl Pts',(8.57112741281372,2.33689888190034,-3.75));
#8174=CARTESIAN_POINT('Ctrl Pts',(8.57112741281372,2.33689888190034,12.75));
#8175=CARTESIAN_POINT('Ctrl Pts',(8.51572283259063,2.33840535058003,-3.75));
#8176=CARTESIAN_POINT('Ctrl Pts',(8.51572283259063,2.33840535058003,12.75));
#8177=CARTESIAN_POINT('Ctrl Pts',(8.46043689627596,2.3392342622836,-3.75));
#8178=CARTESIAN_POINT('Ctrl Pts',(8.46043689627596,2.3392342622836,12.75));
#8179=CARTESIAN_POINT('Ctrl Pts',(8.40527692606173,2.339459611751,-3.75));
#8180=CARTESIAN_POINT('Ctrl Pts',(8.40527692606173,2.339459611751,12.75));
#8181=CARTESIAN_POINT('Ctrl Pts',(8.35029826768635,2.33886640526141,-3.75));
#8182=CARTESIAN_POINT('Ctrl Pts',(8.35029826768635,2.33886640526141,12.75));
#8183=CARTESIAN_POINT('Ctrl Pts',(8.29563322262997,2.33676998946178,-3.75));
#8184=CARTESIAN_POINT('Ctrl Pts',(8.29563322262997,2.33676998946178,12.75));
#8185=CARTESIAN_POINT('Ctrl Pts',(8.24146380440172,2.33217339857873,-3.75));
#8186=CARTESIAN_POINT('Ctrl Pts',(8.24146380440172,2.33217339857873,12.75));
#8187=CARTESIAN_POINT('Ctrl Pts',(8.19867202257947,2.32567282066755,-3.75));
#8188=CARTESIAN_POINT('Ctrl Pts',(8.19867202257947,2.32567282066755,12.75));
#8189=CARTESIAN_POINT('Ctrl Pts',(8.16694940973767,2.31883955953704,-3.75));
#8190=CARTESIAN_POINT('Ctrl Pts',(8.16694940973767,2.31883955953704,12.75));
#8191=CARTESIAN_POINT('Ctrl Pts',(8.14597432907962,2.31336634706602,-3.75));
#8192=CARTESIAN_POINT('Ctrl Pts',(8.14597432907962,2.31336634706602,12.75));
#8193=CARTESIAN_POINT('Ctrl Pts',(8.13553012180811,2.31040030805735,-3.75));
#8194=CARTESIAN_POINT('Ctrl Pts',(8.13553012180811,2.31040030805735,12.75));
#8195=CARTESIAN_POINT('',(11.9792754136349,0.704954299427496,6.));
#8196=CARTESIAN_POINT('Ctrl Pts',(11.9792754136349,0.704954299427529,6.));
#8197=CARTESIAN_POINT('Ctrl Pts',(11.9691386658393,0.714023134927411,6.));
#8198=CARTESIAN_POINT('Ctrl Pts',(11.9488435391885,0.73210763976631,6.));
#8199=CARTESIAN_POINT('Ctrl Pts',(11.9183359560736,0.759074898533419,6.));
#8200=CARTESIAN_POINT('Ctrl Pts',(11.877529348846,0.794712140666325,6.));
#8201=CARTESIAN_POINT('Ctrl Pts',(11.8263046631092,0.838726039995982,6.));
#8202=CARTESIAN_POINT('Ctrl Pts',(11.7748638454684,0.882205904336896,6.));
#8203=CARTESIAN_POINT('Ctrl Pts',(11.7232078225909,0.925149766751161,6.));
#8204=CARTESIAN_POINT('Ctrl Pts',(11.6713384077523,0.967555069553193,6.));
#8205=CARTESIAN_POINT('Ctrl Pts',(11.6192586585895,1.00941863307588,6.));
#8206=CARTESIAN_POINT('Ctrl Pts',(11.5669726710206,1.05073678224334,6.));
#8207=CARTESIAN_POINT('Ctrl Pts',(11.5144851912285,1.09150552381395,6.));
#8208=CARTESIAN_POINT('Ctrl Pts',(11.4618012771636,1.13172071766774,6.));
#8209=CARTESIAN_POINT('Ctrl Pts',(11.4089259705106,1.17137823760545,6.));
#8210=CARTESIAN_POINT('Ctrl Pts',(11.3558638941869,1.21047418192819,6.));
#8211=CARTESIAN_POINT('Ctrl Pts',(11.30261917075,1.24900490126928,6.));
#8212=CARTESIAN_POINT('Ctrl Pts',(11.2491956455455,1.28696685552412,6.));
#8213=CARTESIAN_POINT('Ctrl Pts',(11.1955970312291,1.32435651843207,6.));
#8214=CARTESIAN_POINT('Ctrl Pts',(11.1418270749817,1.36117027439398,6.));
#8215=CARTESIAN_POINT('Ctrl Pts',(11.0878897426906,1.39740430473756,6.));
#8216=CARTESIAN_POINT('Ctrl Pts',(11.033789312906,1.43305454241432,6.));
#8217=CARTESIAN_POINT('Ctrl Pts',(10.9795302662584,1.46811677324654,6.));
#8218=CARTESIAN_POINT('Ctrl Pts',(10.9251172180581,1.50258671261028,6.));
#8219=CARTESIAN_POINT('Ctrl Pts',(10.8705548380775,1.53646008988796,6.));
#8220=CARTESIAN_POINT('Ctrl Pts',(10.8158477697972,1.56973274862052,6.));
#8221=CARTESIAN_POINT('Ctrl Pts',(10.761000572936,1.60240070038749,6.));
#8222=CARTESIAN_POINT('Ctrl Pts',(10.7060177866027,1.63445994423348,6.));
#8223=CARTESIAN_POINT('Ctrl Pts',(10.6509039769739,1.66590631967585,6.));
#8224=CARTESIAN_POINT('Ctrl Pts',(10.59566379085,1.69673535547184,6.));
#8225=CARTESIAN_POINT('Ctrl Pts',(10.5403020105194,1.72694211360792,6.));
#8226=CARTESIAN_POINT('Ctrl Pts',(10.4848236013528,1.75652107004318,6.));
#8227=CARTESIAN_POINT('Ctrl Pts',(10.4292336483793,1.78546643461776,6.));
#8228=CARTESIAN_POINT('Ctrl Pts',(10.3735373011506,1.81377244526718,6.));
#8229=CARTESIAN_POINT('Ctrl Pts',(10.317739716759,1.84143367405762,6.));
#8230=CARTESIAN_POINT('Ctrl Pts',(10.2618460035706,1.86844533887956,6.));
#8231=CARTESIAN_POINT('Ctrl Pts',(10.2058611678956,1.89480360265125,6.));
#8232=CARTESIAN_POINT('Ctrl Pts',(10.1497902344364,1.92050480406378,6.));
#8233=CARTESIAN_POINT('Ctrl Pts',(10.0936383641523,1.94554471072257,6.));
#8234=CARTESIAN_POINT('Ctrl Pts',(10.037410974034,1.96991776698621,6.));
#8235=CARTESIAN_POINT('Ctrl Pts',(9.98111385659409,1.99361634997092,6.));
#8236=CARTESIAN_POINT('Ctrl Pts',(9.92475330165988,2.01663001707736,6.));
#8237=CARTESIAN_POINT('Ctrl Pts',(9.86833584478527,2.03894719582859,6.));
#8238=CARTESIAN_POINT('Ctrl Pts',(9.81186801391803,2.06055689146528,6.));
#8239=CARTESIAN_POINT('Ctrl Pts',(9.75535607889871,2.08145038176732,6.));
#8240=CARTESIAN_POINT('Ctrl Pts',(9.69880579601398,2.10162295100989,6.));
#8241=CARTESIAN_POINT('Ctrl Pts',(9.64222216484242,2.12107554726937,6.));
#8242=CARTESIAN_POINT('Ctrl Pts',(9.58561005875903,2.13981058538587,6.));
#8243=CARTESIAN_POINT('Ctrl Pts',(9.52897485563506,2.15782775391113,6.));
#8244=CARTESIAN_POINT('Ctrl Pts',(9.4723230488593,2.17511995998945,6.));
#8245=CARTESIAN_POINT('Ctrl Pts',(9.41566291502215,2.19166889809876,6.));
#8246=CARTESIAN_POINT('Ctrl Pts',(9.35900502856467,2.2074416540289,6.));
#8247=CARTESIAN_POINT('Ctrl Pts',(9.30236077039477,2.22240082168223,6.));
#8248=CARTESIAN_POINT('Ctrl Pts',(9.24574089753053,2.23651421201962,6.));
#8249=CARTESIAN_POINT('Ctrl Pts',(9.18915420809356,2.24976392906278,6.));
#8250=CARTESIAN_POINT('Ctrl Pts',(9.13260588645235,2.26215759393014,6.));
#8251=CARTESIAN_POINT('Ctrl Pts',(9.07609679780011,2.27373321015996,6.));
#8252=CARTESIAN_POINT('Ctrl Pts',(9.0196273647496,2.28453333318601,6.));
#8253=CARTESIAN_POINT('Ctrl Pts',(8.96320109950669,2.29458154408801,6.));
#8254=CARTESIAN_POINT('Ctrl Pts',(8.90682777405608,2.30386137247017,6.));
#8255=CARTESIAN_POINT('Ctrl Pts',(8.85052793120604,2.31228619203479,6.));
#8256=CARTESIAN_POINT('Ctrl Pts',(8.79433301721166,2.31969862084206,6.));
#8257=CARTESIAN_POINT('Ctrl Pts',(8.73827625692193,2.32593252219559,6.));
#8258=CARTESIAN_POINT('Ctrl Pts',(8.68238458286971,2.33086762045752,6.));
#8259=CARTESIAN_POINT('Ctrl Pts',(8.62667187892838,2.33447589689188,6.));
#8260=CARTESIAN_POINT('Ctrl Pts',(8.57112741281372,2.33689888190034,6.));
#8261=CARTESIAN_POINT('Ctrl Pts',(8.51572283259063,2.33840535058003,6.));
#8262=CARTESIAN_POINT('Ctrl Pts',(8.46043689627596,2.3392342622836,6.));
#8263=CARTESIAN_POINT('Ctrl Pts',(8.40527692606173,2.339459611751,6.));
#8264=CARTESIAN_POINT('Ctrl Pts',(8.35029826768635,2.33886640526141,6.));
#8265=CARTESIAN_POINT('Ctrl Pts',(8.29563322262997,2.33676998946178,6.));
#8266=CARTESIAN_POINT('Ctrl Pts',(8.24146380440172,2.33217339857873,6.));
#8267=CARTESIAN_POINT('Ctrl Pts',(8.19867202257947,2.32567282066755,6.));
#8268=CARTESIAN_POINT('Ctrl Pts',(8.16694940973767,2.31883955953704,6.));
#8269=CARTESIAN_POINT('Ctrl Pts',(8.14597432907962,2.31336634706602,6.));
#8270=CARTESIAN_POINT('Ctrl Pts',(8.13553012180811,2.31040030805735,6.));
#8271=CARTESIAN_POINT('',(11.9792754136349,0.704954299427496,0.));
#8272=CARTESIAN_POINT('Origin',(3.99680288865056E-13,0.,0.));
#8273=CARTESIAN_POINT('',(11.9792754136349,-0.704954299427528,6.));
#8274=CARTESIAN_POINT('Origin',(3.99680288865056E-13,0.,6.));
#8275=CARTESIAN_POINT('',(11.9792754136349,-0.704954299427528,0.));
#8276=CARTESIAN_POINT('Ctrl Pts',(8.13553012180811,-2.31040030805735,-3.75));
#8277=CARTESIAN_POINT('Ctrl Pts',(8.13553012180811,-2.31040030805735,12.75));
#8278=CARTESIAN_POINT('Ctrl Pts',(8.14597432907962,-2.31336634706602,-3.75));
#8279=CARTESIAN_POINT('Ctrl Pts',(8.14597432907962,-2.31336634706602,12.75));
#8280=CARTESIAN_POINT('Ctrl Pts',(8.16694940973767,-2.31883955953704,-3.75));
#8281=CARTESIAN_POINT('Ctrl Pts',(8.16694940973767,-2.31883955953704,12.75));
#8282=CARTESIAN_POINT('Ctrl Pts',(8.19867202257947,-2.32567282066755,-3.75));
#8283=CARTESIAN_POINT('Ctrl Pts',(8.19867202257947,-2.32567282066755,12.75));
#8284=CARTESIAN_POINT('Ctrl Pts',(8.24146380440172,-2.33217339857873,-3.75));
#8285=CARTESIAN_POINT('Ctrl Pts',(8.24146380440172,-2.33217339857873,12.75));
#8286=CARTESIAN_POINT('Ctrl Pts',(8.29563322262997,-2.33676998946178,-3.75));
#8287=CARTESIAN_POINT('Ctrl Pts',(8.29563322262997,-2.33676998946178,12.75));
#8288=CARTESIAN_POINT('Ctrl Pts',(8.35029826768635,-2.33886640526141,-3.75));
#8289=CARTESIAN_POINT('Ctrl Pts',(8.35029826768635,-2.33886640526141,12.75));
#8290=CARTESIAN_POINT('Ctrl Pts',(8.40527692606173,-2.339459611751,-3.75));
#8291=CARTESIAN_POINT('Ctrl Pts',(8.40527692606173,-2.339459611751,12.75));
#8292=CARTESIAN_POINT('Ctrl Pts',(8.46043689627596,-2.3392342622836,-3.75));
#8293=CARTESIAN_POINT('Ctrl Pts',(8.46043689627596,-2.3392342622836,12.75));
#8294=CARTESIAN_POINT('Ctrl Pts',(8.51572283259063,-2.33840535058003,-3.75));
#8295=CARTESIAN_POINT('Ctrl Pts',(8.51572283259063,-2.33840535058003,12.75));
#8296=CARTESIAN_POINT('Ctrl Pts',(8.57112741281372,-2.33689888190034,-3.75));
#8297=CARTESIAN_POINT('Ctrl Pts',(8.57112741281372,-2.33689888190034,12.75));
#8298=CARTESIAN_POINT('Ctrl Pts',(8.62667187892838,-2.33447589689188,-3.75));
#8299=CARTESIAN_POINT('Ctrl Pts',(8.62667187892838,-2.33447589689188,12.75));
#8300=CARTESIAN_POINT('Ctrl Pts',(8.68238458286971,-2.33086762045752,-3.75));
#8301=CARTESIAN_POINT('Ctrl Pts',(8.68238458286971,-2.33086762045752,12.75));
#8302=CARTESIAN_POINT('Ctrl Pts',(8.73827625692193,-2.32593252219559,-3.75));
#8303=CARTESIAN_POINT('Ctrl Pts',(8.73827625692193,-2.32593252219559,12.75));
#8304=CARTESIAN_POINT('Ctrl Pts',(8.79433301721166,-2.31969862084206,-3.75));
#8305=CARTESIAN_POINT('Ctrl Pts',(8.79433301721166,-2.31969862084206,12.75));
#8306=CARTESIAN_POINT('Ctrl Pts',(8.85052793120604,-2.31228619203479,-3.75));
#8307=CARTESIAN_POINT('Ctrl Pts',(8.85052793120604,-2.31228619203479,12.75));
#8308=CARTESIAN_POINT('Ctrl Pts',(8.90682777405608,-2.30386137247017,-3.75));
#8309=CARTESIAN_POINT('Ctrl Pts',(8.90682777405608,-2.30386137247017,12.75));
#8310=CARTESIAN_POINT('Ctrl Pts',(8.96320109950669,-2.29458154408801,-3.75));
#8311=CARTESIAN_POINT('Ctrl Pts',(8.96320109950669,-2.29458154408801,12.75));
#8312=CARTESIAN_POINT('Ctrl Pts',(9.0196273647496,-2.28453333318601,-3.75));
#8313=CARTESIAN_POINT('Ctrl Pts',(9.0196273647496,-2.28453333318601,12.75));
#8314=CARTESIAN_POINT('Ctrl Pts',(9.07609679780011,-2.27373321015996,-3.75));
#8315=CARTESIAN_POINT('Ctrl Pts',(9.07609679780011,-2.27373321015996,12.75));
#8316=CARTESIAN_POINT('Ctrl Pts',(9.13260588645235,-2.26215759393014,-3.75));
#8317=CARTESIAN_POINT('Ctrl Pts',(9.13260588645235,-2.26215759393014,12.75));
#8318=CARTESIAN_POINT('Ctrl Pts',(9.18915420809356,-2.24976392906278,-3.75));
#8319=CARTESIAN_POINT('Ctrl Pts',(9.18915420809356,-2.24976392906278,12.75));
#8320=CARTESIAN_POINT('Ctrl Pts',(9.24574089753053,-2.23651421201962,-3.75));
#8321=CARTESIAN_POINT('Ctrl Pts',(9.24574089753053,-2.23651421201962,12.75));
#8322=CARTESIAN_POINT('Ctrl Pts',(9.30236077039477,-2.22240082168223,-3.75));
#8323=CARTESIAN_POINT('Ctrl Pts',(9.30236077039477,-2.22240082168223,12.75));
#8324=CARTESIAN_POINT('Ctrl Pts',(9.35900502856467,-2.2074416540289,-3.75));
#8325=CARTESIAN_POINT('Ctrl Pts',(9.35900502856467,-2.2074416540289,12.75));
#8326=CARTESIAN_POINT('Ctrl Pts',(9.41566291502215,-2.19166889809876,-3.75));
#8327=CARTESIAN_POINT('Ctrl Pts',(9.41566291502215,-2.19166889809876,12.75));
#8328=CARTESIAN_POINT('Ctrl Pts',(9.4723230488593,-2.17511995998945,-3.75));
#8329=CARTESIAN_POINT('Ctrl Pts',(9.4723230488593,-2.17511995998945,12.75));
#8330=CARTESIAN_POINT('Ctrl Pts',(9.52897485563506,-2.15782775391113,-3.75));
#8331=CARTESIAN_POINT('Ctrl Pts',(9.52897485563506,-2.15782775391113,12.75));
#8332=CARTESIAN_POINT('Ctrl Pts',(9.58561005875903,-2.13981058538587,-3.75));
#8333=CARTESIAN_POINT('Ctrl Pts',(9.58561005875903,-2.13981058538587,12.75));
#8334=CARTESIAN_POINT('Ctrl Pts',(9.64222216484242,-2.12107554726937,-3.75));
#8335=CARTESIAN_POINT('Ctrl Pts',(9.64222216484242,-2.12107554726937,12.75));
#8336=CARTESIAN_POINT('Ctrl Pts',(9.69880579601398,-2.10162295100989,-3.75));
#8337=CARTESIAN_POINT('Ctrl Pts',(9.69880579601398,-2.10162295100989,12.75));
#8338=CARTESIAN_POINT('Ctrl Pts',(9.75535607889871,-2.08145038176732,-3.75));
#8339=CARTESIAN_POINT('Ctrl Pts',(9.75535607889871,-2.08145038176732,12.75));
#8340=CARTESIAN_POINT('Ctrl Pts',(9.81186801391803,-2.06055689146528,-3.75));
#8341=CARTESIAN_POINT('Ctrl Pts',(9.81186801391803,-2.06055689146528,12.75));
#8342=CARTESIAN_POINT('Ctrl Pts',(9.86833584478527,-2.03894719582859,-3.75));
#8343=CARTESIAN_POINT('Ctrl Pts',(9.86833584478527,-2.03894719582859,12.75));
#8344=CARTESIAN_POINT('Ctrl Pts',(9.92475330165988,-2.01663001707736,-3.75));
#8345=CARTESIAN_POINT('Ctrl Pts',(9.92475330165988,-2.01663001707736,12.75));
#8346=CARTESIAN_POINT('Ctrl Pts',(9.98111385659409,-1.99361634997092,-3.75));
#8347=CARTESIAN_POINT('Ctrl Pts',(9.98111385659409,-1.99361634997092,12.75));
#8348=CARTESIAN_POINT('Ctrl Pts',(10.037410974034,-1.96991776698621,-3.75));
#8349=CARTESIAN_POINT('Ctrl Pts',(10.037410974034,-1.96991776698621,12.75));
#8350=CARTESIAN_POINT('Ctrl Pts',(10.0936383641523,-1.94554471072257,-3.75));
#8351=CARTESIAN_POINT('Ctrl Pts',(10.0936383641523,-1.94554471072257,12.75));
#8352=CARTESIAN_POINT('Ctrl Pts',(10.1497902344364,-1.92050480406378,-3.75));
#8353=CARTESIAN_POINT('Ctrl Pts',(10.1497902344364,-1.92050480406378,12.75));
#8354=CARTESIAN_POINT('Ctrl Pts',(10.2058611678956,-1.89480360265125,-3.75));
#8355=CARTESIAN_POINT('Ctrl Pts',(10.2058611678956,-1.89480360265125,12.75));
#8356=CARTESIAN_POINT('Ctrl Pts',(10.2618460035706,-1.86844533887956,-3.75));
#8357=CARTESIAN_POINT('Ctrl Pts',(10.2618460035706,-1.86844533887956,12.75));
#8358=CARTESIAN_POINT('Ctrl Pts',(10.317739716759,-1.84143367405762,-3.75));
#8359=CARTESIAN_POINT('Ctrl Pts',(10.317739716759,-1.84143367405762,12.75));
#8360=CARTESIAN_POINT('Ctrl Pts',(10.3735373011506,-1.81377244526718,-3.75));
#8361=CARTESIAN_POINT('Ctrl Pts',(10.3735373011506,-1.81377244526718,12.75));
#8362=CARTESIAN_POINT('Ctrl Pts',(10.4292336483793,-1.78546643461776,-3.75));
#8363=CARTESIAN_POINT('Ctrl Pts',(10.4292336483793,-1.78546643461776,12.75));
#8364=CARTESIAN_POINT('Ctrl Pts',(10.4848236013528,-1.75652107004318,-3.75));
#8365=CARTESIAN_POINT('Ctrl Pts',(10.4848236013528,-1.75652107004318,12.75));
#8366=CARTESIAN_POINT('Ctrl Pts',(10.5403020105194,-1.72694211360792,-3.75));
#8367=CARTESIAN_POINT('Ctrl Pts',(10.5403020105194,-1.72694211360792,12.75));
#8368=CARTESIAN_POINT('Ctrl Pts',(10.59566379085,-1.69673535547184,-3.75));
#8369=CARTESIAN_POINT('Ctrl Pts',(10.59566379085,-1.69673535547184,12.75));
#8370=CARTESIAN_POINT('Ctrl Pts',(10.6509039769739,-1.66590631967585,-3.75));
#8371=CARTESIAN_POINT('Ctrl Pts',(10.6509039769739,-1.66590631967585,12.75));
#8372=CARTESIAN_POINT('Ctrl Pts',(10.7060177866027,-1.63445994423348,-3.75));
#8373=CARTESIAN_POINT('Ctrl Pts',(10.7060177866027,-1.63445994423348,12.75));
#8374=CARTESIAN_POINT('Ctrl Pts',(10.761000572936,-1.60240070038749,-3.75));
#8375=CARTESIAN_POINT('Ctrl Pts',(10.761000572936,-1.60240070038749,12.75));
#8376=CARTESIAN_POINT('Ctrl Pts',(10.8158477697972,-1.56973274862052,-3.75));
#8377=CARTESIAN_POINT('Ctrl Pts',(10.8158477697972,-1.56973274862052,12.75));
#8378=CARTESIAN_POINT('Ctrl Pts',(10.8705548380775,-1.53646008988796,-3.75));
#8379=CARTESIAN_POINT('Ctrl Pts',(10.8705548380775,-1.53646008988796,12.75));
#8380=CARTESIAN_POINT('Ctrl Pts',(10.9251172180581,-1.50258671261028,-3.75));
#8381=CARTESIAN_POINT('Ctrl Pts',(10.9251172180581,-1.50258671261028,12.75));
#8382=CARTESIAN_POINT('Ctrl Pts',(10.9795302662584,-1.46811677324654,-3.75));
#8383=CARTESIAN_POINT('Ctrl Pts',(10.9795302662584,-1.46811677324654,12.75));
#8384=CARTESIAN_POINT('Ctrl Pts',(11.033789312906,-1.43305454241432,-3.75));
#8385=CARTESIAN_POINT('Ctrl Pts',(11.033789312906,-1.43305454241432,12.75));
#8386=CARTESIAN_POINT('Ctrl Pts',(11.0878897426906,-1.39740430473756,-3.75));
#8387=CARTESIAN_POINT('Ctrl Pts',(11.0878897426906,-1.39740430473756,12.75));
#8388=CARTESIAN_POINT('Ctrl Pts',(11.1418270749817,-1.36117027439398,-3.75));
#8389=CARTESIAN_POINT('Ctrl Pts',(11.1418270749817,-1.36117027439398,12.75));
#8390=CARTESIAN_POINT('Ctrl Pts',(11.1955970312291,-1.32435651843207,-3.75));
#8391=CARTESIAN_POINT('Ctrl Pts',(11.1955970312291,-1.32435651843207,12.75));
#8392=CARTESIAN_POINT('Ctrl Pts',(11.2491956455455,-1.28696685552412,-3.75));
#8393=CARTESIAN_POINT('Ctrl Pts',(11.2491956455455,-1.28696685552412,12.75));
#8394=CARTESIAN_POINT('Ctrl Pts',(11.30261917075,-1.24900490126928,-3.75));
#8395=CARTESIAN_POINT('Ctrl Pts',(11.30261917075,-1.24900490126928,12.75));
#8396=CARTESIAN_POINT('Ctrl Pts',(11.3558638941869,-1.21047418192819,-3.75));
#8397=CARTESIAN_POINT('Ctrl Pts',(11.3558638941869,-1.21047418192819,12.75));
#8398=CARTESIAN_POINT('Ctrl Pts',(11.4089259705106,-1.17137823760545,-3.75));
#8399=CARTESIAN_POINT('Ctrl Pts',(11.4089259705106,-1.17137823760545,12.75));
#8400=CARTESIAN_POINT('Ctrl Pts',(11.4618012771636,-1.13172071766774,-3.75));
#8401=CARTESIAN_POINT('Ctrl Pts',(11.4618012771636,-1.13172071766774,12.75));
#8402=CARTESIAN_POINT('Ctrl Pts',(11.5144851912285,-1.09150552381395,-3.75));
#8403=CARTESIAN_POINT('Ctrl Pts',(11.5144851912285,-1.09150552381395,12.75));
#8404=CARTESIAN_POINT('Ctrl Pts',(11.5669726710206,-1.05073678224334,-3.75));
#8405=CARTESIAN_POINT('Ctrl Pts',(11.5669726710206,-1.05073678224334,12.75));
#8406=CARTESIAN_POINT('Ctrl Pts',(11.6192586585895,-1.00941863307588,-3.75));
#8407=CARTESIAN_POINT('Ctrl Pts',(11.6192586585895,-1.00941863307588,12.75));
#8408=CARTESIAN_POINT('Ctrl Pts',(11.6713384077523,-0.967555069553193,-3.75));
#8409=CARTESIAN_POINT('Ctrl Pts',(11.6713384077523,-0.967555069553193,12.75));
#8410=CARTESIAN_POINT('Ctrl Pts',(11.7232078225909,-0.925149766751161,-3.75));
#8411=CARTESIAN_POINT('Ctrl Pts',(11.7232078225909,-0.925149766751161,12.75));
#8412=CARTESIAN_POINT('Ctrl Pts',(11.7748638454684,-0.882205904336896,-3.75));
#8413=CARTESIAN_POINT('Ctrl Pts',(11.7748638454684,-0.882205904336896,12.75));
#8414=CARTESIAN_POINT('Ctrl Pts',(11.8263046631092,-0.838726039995982,-3.75));
#8415=CARTESIAN_POINT('Ctrl Pts',(11.8263046631092,-0.838726039995982,12.75));
#8416=CARTESIAN_POINT('Ctrl Pts',(11.877529348846,-0.794712140666325,-3.75));
#8417=CARTESIAN_POINT('Ctrl Pts',(11.877529348846,-0.794712140666325,12.75));
#8418=CARTESIAN_POINT('Ctrl Pts',(11.9183359560736,-0.759074898533419,-3.75));
#8419=CARTESIAN_POINT('Ctrl Pts',(11.9183359560736,-0.759074898533419,12.75));
#8420=CARTESIAN_POINT('Ctrl Pts',(11.9488435391885,-0.73210763976631,-3.75));
#8421=CARTESIAN_POINT('Ctrl Pts',(11.9488435391885,-0.73210763976631,12.75));
#8422=CARTESIAN_POINT('Ctrl Pts',(11.9691386658393,-0.714023134927411,-3.75));
#8423=CARTESIAN_POINT('Ctrl Pts',(11.9691386658393,-0.714023134927411,12.75));
#8424=CARTESIAN_POINT('Ctrl Pts',(11.9792754136349,-0.704954299427529,-3.75));
#8425=CARTESIAN_POINT('Ctrl Pts',(11.9792754136349,-0.704954299427529,12.75));
#8426=CARTESIAN_POINT('Ctrl Pts',(8.13553012180811,-2.31040030805735,6.));
#8427=CARTESIAN_POINT('Ctrl Pts',(8.14597432907962,-2.31336634706602,6.));
#8428=CARTESIAN_POINT('Ctrl Pts',(8.16694940973767,-2.31883955953704,6.));
#8429=CARTESIAN_POINT('Ctrl Pts',(8.19867202257947,-2.32567282066755,6.));
#8430=CARTESIAN_POINT('Ctrl Pts',(8.24146380440172,-2.33217339857873,6.));
#8431=CARTESIAN_POINT('Ctrl Pts',(8.29563322262997,-2.33676998946178,6.));
#8432=CARTESIAN_POINT('Ctrl Pts',(8.35029826768635,-2.33886640526141,6.));
#8433=CARTESIAN_POINT('Ctrl Pts',(8.40527692606173,-2.339459611751,6.));
#8434=CARTESIAN_POINT('Ctrl Pts',(8.46043689627596,-2.3392342622836,6.));
#8435=CARTESIAN_POINT('Ctrl Pts',(8.51572283259063,-2.33840535058003,6.));
#8436=CARTESIAN_POINT('Ctrl Pts',(8.57112741281372,-2.33689888190034,6.));
#8437=CARTESIAN_POINT('Ctrl Pts',(8.62667187892838,-2.33447589689188,6.));
#8438=CARTESIAN_POINT('Ctrl Pts',(8.68238458286971,-2.33086762045752,6.));
#8439=CARTESIAN_POINT('Ctrl Pts',(8.73827625692193,-2.32593252219559,6.));
#8440=CARTESIAN_POINT('Ctrl Pts',(8.79433301721166,-2.31969862084206,6.));
#8441=CARTESIAN_POINT('Ctrl Pts',(8.85052793120604,-2.31228619203479,6.));
#8442=CARTESIAN_POINT('Ctrl Pts',(8.90682777405608,-2.30386137247017,6.));
#8443=CARTESIAN_POINT('Ctrl Pts',(8.96320109950669,-2.29458154408801,6.));
#8444=CARTESIAN_POINT('Ctrl Pts',(9.0196273647496,-2.28453333318601,6.));
#8445=CARTESIAN_POINT('Ctrl Pts',(9.07609679780011,-2.27373321015996,6.));
#8446=CARTESIAN_POINT('Ctrl Pts',(9.13260588645235,-2.26215759393014,6.));
#8447=CARTESIAN_POINT('Ctrl Pts',(9.18915420809356,-2.24976392906278,6.));
#8448=CARTESIAN_POINT('Ctrl Pts',(9.24574089753053,-2.23651421201962,6.));
#8449=CARTESIAN_POINT('Ctrl Pts',(9.30236077039477,-2.22240082168223,6.));
#8450=CARTESIAN_POINT('Ctrl Pts',(9.35900502856467,-2.2074416540289,6.));
#8451=CARTESIAN_POINT('Ctrl Pts',(9.41566291502215,-2.19166889809876,6.));
#8452=CARTESIAN_POINT('Ctrl Pts',(9.4723230488593,-2.17511995998945,6.));
#8453=CARTESIAN_POINT('Ctrl Pts',(9.52897485563506,-2.15782775391113,6.));
#8454=CARTESIAN_POINT('Ctrl Pts',(9.58561005875903,-2.13981058538587,6.));
#8455=CARTESIAN_POINT('Ctrl Pts',(9.64222216484242,-2.12107554726937,6.));
#8456=CARTESIAN_POINT('Ctrl Pts',(9.69880579601398,-2.10162295100989,6.));
#8457=CARTESIAN_POINT('Ctrl Pts',(9.75535607889871,-2.08145038176732,6.));
#8458=CARTESIAN_POINT('Ctrl Pts',(9.81186801391803,-2.06055689146528,6.));
#8459=CARTESIAN_POINT('Ctrl Pts',(9.86833584478527,-2.03894719582859,6.));
#8460=CARTESIAN_POINT('Ctrl Pts',(9.92475330165988,-2.01663001707736,6.));
#8461=CARTESIAN_POINT('Ctrl Pts',(9.98111385659409,-1.99361634997092,6.));
#8462=CARTESIAN_POINT('Ctrl Pts',(10.037410974034,-1.96991776698621,6.));
#8463=CARTESIAN_POINT('Ctrl Pts',(10.0936383641523,-1.94554471072257,6.));
#8464=CARTESIAN_POINT('Ctrl Pts',(10.1497902344364,-1.92050480406378,6.));
#8465=CARTESIAN_POINT('Ctrl Pts',(10.2058611678956,-1.89480360265125,6.));
#8466=CARTESIAN_POINT('Ctrl Pts',(10.2618460035706,-1.86844533887956,6.));
#8467=CARTESIAN_POINT('Ctrl Pts',(10.317739716759,-1.84143367405762,6.));
#8468=CARTESIAN_POINT('Ctrl Pts',(10.3735373011506,-1.81377244526718,6.));
#8469=CARTESIAN_POINT('Ctrl Pts',(10.4292336483793,-1.78546643461776,6.));
#8470=CARTESIAN_POINT('Ctrl Pts',(10.4848236013528,-1.75652107004318,6.));
#8471=CARTESIAN_POINT('Ctrl Pts',(10.5403020105194,-1.72694211360792,6.));
#8472=CARTESIAN_POINT('Ctrl Pts',(10.59566379085,-1.69673535547184,6.));
#8473=CARTESIAN_POINT('Ctrl Pts',(10.6509039769739,-1.66590631967585,6.));
#8474=CARTESIAN_POINT('Ctrl Pts',(10.7060177866027,-1.63445994423348,6.));
#8475=CARTESIAN_POINT('Ctrl Pts',(10.761000572936,-1.60240070038749,6.));
#8476=CARTESIAN_POINT('Ctrl Pts',(10.8158477697972,-1.56973274862052,6.));
#8477=CARTESIAN_POINT('Ctrl Pts',(10.8705548380775,-1.53646008988796,6.));
#8478=CARTESIAN_POINT('Ctrl Pts',(10.9251172180581,-1.50258671261028,6.));
#8479=CARTESIAN_POINT('Ctrl Pts',(10.9795302662584,-1.46811677324654,6.));
#8480=CARTESIAN_POINT('Ctrl Pts',(11.033789312906,-1.43305454241432,6.));
#8481=CARTESIAN_POINT('Ctrl Pts',(11.0878897426906,-1.39740430473756,6.));
#8482=CARTESIAN_POINT('Ctrl Pts',(11.1418270749817,-1.36117027439398,6.));
#8483=CARTESIAN_POINT('Ctrl Pts',(11.1955970312291,-1.32435651843207,6.));
#8484=CARTESIAN_POINT('Ctrl Pts',(11.2491956455455,-1.28696685552412,6.));
#8485=CARTESIAN_POINT('Ctrl Pts',(11.30261917075,-1.24900490126928,6.));
#8486=CARTESIAN_POINT('Ctrl Pts',(11.3558638941869,-1.21047418192819,6.));
#8487=CARTESIAN_POINT('Ctrl Pts',(11.4089259705106,-1.17137823760545,6.));
#8488=CARTESIAN_POINT('Ctrl Pts',(11.4618012771636,-1.13172071766774,6.));
#8489=CARTESIAN_POINT('Ctrl Pts',(11.5144851912285,-1.09150552381395,6.));
#8490=CARTESIAN_POINT('Ctrl Pts',(11.5669726710206,-1.05073678224334,6.));
#8491=CARTESIAN_POINT('Ctrl Pts',(11.6192586585895,-1.00941863307588,6.));
#8492=CARTESIAN_POINT('Ctrl Pts',(11.6713384077523,-0.967555069553193,6.));
#8493=CARTESIAN_POINT('Ctrl Pts',(11.7232078225909,-0.925149766751161,6.));
#8494=CARTESIAN_POINT('Ctrl Pts',(11.7748638454684,-0.882205904336896,6.));
#8495=CARTESIAN_POINT('Ctrl Pts',(11.8263046631092,-0.838726039995982,6.));
#8496=CARTESIAN_POINT('Ctrl Pts',(11.877529348846,-0.794712140666325,6.));
#8497=CARTESIAN_POINT('Ctrl Pts',(11.9183359560736,-0.759074898533419,6.));
#8498=CARTESIAN_POINT('Ctrl Pts',(11.9488435391885,-0.73210763976631,6.));
#8499=CARTESIAN_POINT('Ctrl Pts',(11.9691386658393,-0.714023134927411,6.));
#8500=CARTESIAN_POINT('Ctrl Pts',(11.9792754136349,-0.704954299427529,6.));
#8501=CARTESIAN_POINT('Origin',(0.,0.,6.));
#8502=CARTESIAN_POINT('Origin',(0.,0.,6.));
#8503=CARTESIAN_POINT('',(-5.,6.12323399573677E-16,6.));
#8504=CARTESIAN_POINT('Origin',(0.,0.,6.));
#8505=CARTESIAN_POINT('Origin',(0.,0.,0.));
#8506=CARTESIAN_POINT('',(-5.,-6.12323399573677E-16,0.));
#8507=CARTESIAN_POINT('Origin',(0.,0.,0.));
#8508=CARTESIAN_POINT('',(0.,0.,0.));
#8509=CARTESIAN_POINT('Origin',(0.,-6.,9.));
#8510=CARTESIAN_POINT('',(1.,-6.,9.));
#8511=CARTESIAN_POINT('',(-1.,-6.,9.));
#8512=CARTESIAN_POINT('Origin',(0.,-6.,9.));
#8513=CARTESIAN_POINT('Origin',(0.,-6.,9.));
#8514=CARTESIAN_POINT('',(-1.,-6.92820323027551,9.));
#8515=CARTESIAN_POINT('',(-1.,-6.,9.));
#8516=CARTESIAN_POINT('',(1.,-6.92820323027551,9.));
#8517=CARTESIAN_POINT('Ctrl Pts',(1.,-6.92820323027551,9.));
#8518=CARTESIAN_POINT('Ctrl Pts',(1.,-6.92820323027551,8.87425193147876));
#8519=CARTESIAN_POINT('Ctrl Pts',(0.974833943897391,-6.93198034025289,8.74024144192777));
#8520=CARTESIAN_POINT('Ctrl Pts',(0.872727208600932,-6.94557411965751,8.49391406486289));
#8521=CARTESIAN_POINT('Ctrl Pts',(0.795795807000654,-6.95518913236708,8.38158224462756));
#8522=CARTESIAN_POINT('Ctrl Pts',(0.618419025069236,-6.97319901589886,8.20420546269614));
#8523=CARTESIAN_POINT('Ctrl Pts',(0.506086655807109,-6.98277103675548,8.12727306529771));
#8524=CARTESIAN_POINT('Ctrl Pts',(0.259757407800085,-6.99626622874452,8.02516560412687));
#8525=CARTESIAN_POINT('Ctrl Pts',(0.125746268276869,-7.,8.));
#8526=CARTESIAN_POINT('Ctrl Pts',(-0.125746268276869,-7.,8.));
#8527=CARTESIAN_POINT('Ctrl Pts',(-0.259757407800085,-6.99626622874452,
8.02516560412687));
#8528=CARTESIAN_POINT('Ctrl Pts',(-0.506086655807109,-6.98277103675548,
8.12727306529771));
#8529=CARTESIAN_POINT('Ctrl Pts',(-0.618419025069236,-6.97319901589886,
8.20420546269614));
#8530=CARTESIAN_POINT('Ctrl Pts',(-0.795795807000653,-6.95518913236708,
8.38158224462756));
#8531=CARTESIAN_POINT('Ctrl Pts',(-0.872727208600933,-6.94557411965751,
8.49391406486289));
#8532=CARTESIAN_POINT('Ctrl Pts',(-0.974833943897392,-6.93198034025289,
8.74024144192777));
#8533=CARTESIAN_POINT('Ctrl Pts',(-1.,-6.92820323027551,8.87425193147876));
#8534=CARTESIAN_POINT('Ctrl Pts',(-1.,-6.92820323027551,9.));
#8535=CARTESIAN_POINT('Ctrl Pts',(-1.,-6.92820323027551,9.));
#8536=CARTESIAN_POINT('Ctrl Pts',(-1.,-6.92820323027551,9.12574806852124));
#8537=CARTESIAN_POINT('Ctrl Pts',(-0.974833943897391,-6.93198034025289,
9.25975855807223));
#8538=CARTESIAN_POINT('Ctrl Pts',(-0.872727208600932,-6.94557411965751,
9.50608593513711));
#8539=CARTESIAN_POINT('Ctrl Pts',(-0.795795807000653,-6.95518913236708,
9.61841775537244));
#8540=CARTESIAN_POINT('Ctrl Pts',(-0.618419025069235,-6.97319901589886,
9.79579453730386));
#8541=CARTESIAN_POINT('Ctrl Pts',(-0.506086655807108,-6.98277103675548,
9.87272693470229));
#8542=CARTESIAN_POINT('Ctrl Pts',(-0.259757407800085,-6.99626622874452,
9.97483439587313));
#8543=CARTESIAN_POINT('Ctrl Pts',(-0.125746268276869,-7.,10.));
#8544=CARTESIAN_POINT('Ctrl Pts',(0.125746268276869,-7.,10.));
#8545=CARTESIAN_POINT('Ctrl Pts',(0.259757407800085,-6.99626622874452,9.97483439587313));
#8546=CARTESIAN_POINT('Ctrl Pts',(0.506086655807109,-6.98277103675548,9.87272693470229));
#8547=CARTESIAN_POINT('Ctrl Pts',(0.618419025069235,-6.97319901589886,9.79579453730386));
#8548=CARTESIAN_POINT('Ctrl Pts',(0.795795807000653,-6.95518913236708,9.61841775537244));
#8549=CARTESIAN_POINT('Ctrl Pts',(0.872727208600933,-6.94557411965751,9.50608593513711));
#8550=CARTESIAN_POINT('Ctrl Pts',(0.974833943897392,-6.93198034025289,9.25975855807223));
#8551=CARTESIAN_POINT('Ctrl Pts',(1.,-6.92820323027551,9.12574806852124));
#8552=CARTESIAN_POINT('Ctrl Pts',(1.,-6.92820323027551,9.));
#8553=CARTESIAN_POINT('Origin',(0.,-6.,10.5));
#8554=CARTESIAN_POINT('',(1.,-6.,6.5));
#8555=CARTESIAN_POINT('',(1.,-6.,14.5));
#8556=CARTESIAN_POINT('',(-1.,-6.,6.5));
#8557=CARTESIAN_POINT('Origin',(0.,-6.,6.5));
#8558=CARTESIAN_POINT('',(-1.,-6.,6.5));
#8559=CARTESIAN_POINT('Origin',(0.,-6.,10.5));
#8560=CARTESIAN_POINT('',(-1.,-6.,12.));
#8561=CARTESIAN_POINT('',(-1.,-6.,6.5));
#8562=CARTESIAN_POINT('',(1.,-6.,12.));
#8563=CARTESIAN_POINT('',(0.,-6.,12.));
#8564=CARTESIAN_POINT('',(1.,-6.,14.5));
#8565=CARTESIAN_POINT('Origin',(0.,0.,6.5));
#8566=CARTESIAN_POINT('',(-1.,-4.89897948556636,6.5));
#8567=CARTESIAN_POINT('',(1.,-4.89897948556636,6.5));
#8568=CARTESIAN_POINT('Ctrl Pts',(-1.,-4.89897948556636,6.5));
#8569=CARTESIAN_POINT('Ctrl Pts',(-1.,-4.89897948556636,6.3740682480366));
#8570=CARTESIAN_POINT('Ctrl Pts',(-0.974762796248615,-4.90433876618447,
6.23998222283811));
#8571=CARTESIAN_POINT('Ctrl Pts',(-0.872605417648384,-4.92354150792771,
5.99370799496995));
#8572=CARTESIAN_POINT('Ctrl Pts',(-0.795703102192089,-4.93709085101933,
5.88148953981899));
#8573=CARTESIAN_POINT('Ctrl Pts',(-0.618515424645094,-4.96240337638318,
5.704301862272));
#8574=CARTESIAN_POINT('Ctrl Pts',(-0.506294861197626,-4.97583347151864,
5.62739565845524));
#8575=CARTESIAN_POINT('Ctrl Pts',(-0.260013306081865,-4.99476188647081,
5.52523545776417));
#8576=CARTESIAN_POINT('Ctrl Pts',(-0.1259246954214,-5.,5.5));
#8577=CARTESIAN_POINT('Ctrl Pts',(0.125924695421399,-5.,5.5));
#8578=CARTESIAN_POINT('Ctrl Pts',(0.260013306081865,-4.99476188647081,5.52523545776417));
#8579=CARTESIAN_POINT('Ctrl Pts',(0.506294861197626,-4.97583347151864,5.62739565845524));
#8580=CARTESIAN_POINT('Ctrl Pts',(0.618515424645094,-4.96240337638318,5.704301862272));
#8581=CARTESIAN_POINT('Ctrl Pts',(0.795703102192088,-4.93709085101933,5.88148953981899));
#8582=CARTESIAN_POINT('Ctrl Pts',(0.872605417648382,-4.92354150792771,5.99370799496995));
#8583=CARTESIAN_POINT('Ctrl Pts',(0.974762796248614,-4.90433876618447,6.23998222283811));
#8584=CARTESIAN_POINT('Ctrl Pts',(1.,-4.89897948556636,6.3740682480366));
#8585=CARTESIAN_POINT('Ctrl Pts',(1.,-4.89897948556636,6.5));
#8586=CARTESIAN_POINT('',(-1.,0.,6.5));
#8587=CARTESIAN_POINT('',(1.,0.,6.5));
#8588=CARTESIAN_POINT('Origin',(1.,0.,6.5));
#8589=CARTESIAN_POINT('',(1.,-4.89897948556636,12.));
#8590=CARTESIAN_POINT('',(1.,-4.89897948556636,5.));
#8591=CARTESIAN_POINT('',(1.,0.,12.));
#8592=CARTESIAN_POINT('Origin',(-1.,0.,14.5));
#8593=CARTESIAN_POINT('',(-1.,-4.89897948556636,12.));
#8594=CARTESIAN_POINT('',(-1.,-4.89897948556636,5.));
#8595=CARTESIAN_POINT('',(-1.,0.,12.));
#8596=CARTESIAN_POINT('Origin',(0.,0.,5.));
#8597=CARTESIAN_POINT('',(-5.,-6.12323399573677E-16,5.));
#8598=CARTESIAN_POINT('Origin',(0.,0.,5.));
#8599=CARTESIAN_POINT('',(-5.,-6.12323399573677E-16,12.));
#8600=CARTESIAN_POINT('',(-5.,-6.12323399573677E-16,5.));
#8601=CARTESIAN_POINT('Origin',(0.,0.,12.));
#8602=CARTESIAN_POINT('Origin',(0.,0.,12.));
#8603=CARTESIAN_POINT('Origin',(0.,0.,5.));
#8604=CARTESIAN_POINT('',(11.9792754136349,-0.704954299427529,5.));
#8605=CARTESIAN_POINT('',(11.9792754136349,-0.704954299427527,0.2));
#8606=CARTESIAN_POINT('',(11.9792754136349,-0.704954299427529,5.));
#8607=CARTESIAN_POINT('',(5.37912937500617,10.726833976852,5.));
#8608=CARTESIAN_POINT('Origin',(0.,0.,5.));
#8609=CARTESIAN_POINT('',(5.37912937500618,10.726833976852,0.2));
#8610=CARTESIAN_POINT('',(5.37912937500617,10.726833976852,5.));
#8611=CARTESIAN_POINT('Origin',(0.,0.,0.2));
#8612=CARTESIAN_POINT('Origin',(0.,0.,5.));
#8613=CARTESIAN_POINT('',(-11.9792754136349,-0.704954299427521,5.));
#8614=CARTESIAN_POINT('',(-11.9792754136349,-0.704954299427494,0.2));
#8615=CARTESIAN_POINT('',(-11.9792754136349,-0.704954299427521,5.));
#8616=CARTESIAN_POINT('',(-5.37912937500617,10.726833976852,0.2));
#8617=CARTESIAN_POINT('Origin',(0.,0.,0.2));
#8618=CARTESIAN_POINT('',(-5.37912937500617,10.726833976852,5.));
#8619=CARTESIAN_POINT('',(-5.37912937500617,10.726833976852,5.));
#8620=CARTESIAN_POINT('Origin',(0.,0.,5.));
#8621=CARTESIAN_POINT('Origin',(0.,0.,5.));
#8622=CARTESIAN_POINT('',(6.60014603862876,-10.0218796774244,5.));
#8623=CARTESIAN_POINT('',(6.60014603862877,-10.0218796774244,0.2));
#8624=CARTESIAN_POINT('',(6.60014603862876,-10.0218796774244,5.));
#8625=CARTESIAN_POINT('',(-6.60014603862878,-10.0218796774244,0.2));
#8626=CARTESIAN_POINT('Origin',(0.,0.,0.2));
#8627=CARTESIAN_POINT('',(-6.60014603862878,-10.0218796774244,5.));
#8628=CARTESIAN_POINT('',(-6.60014603862878,-10.0218796774244,5.));
#8629=CARTESIAN_POINT('Origin',(0.,0.,5.));
#8630=CARTESIAN_POINT('Origin',(0.,0.,0.2));
#8631=CARTESIAN_POINT('',(-13.5,-1.66533453693773E-15,0.2));
#8632=CARTESIAN_POINT('Origin',(0.,0.,0.2));
#8633=CARTESIAN_POINT('Origin',(0.,0.,0.2));
#8634=CARTESIAN_POINT('Origin',(0.,0.,0.2));
#8635=CARTESIAN_POINT('Origin',(0.,0.,0.2));
#8636=CARTESIAN_POINT('Origin',(0.,0.,5.));
#8637=CARTESIAN_POINT('',(-11.9792754136349,-0.70495429942752,-1.5));
#8638=CARTESIAN_POINT('',(-11.9792754136349,-0.704954299427521,5.));
#8639=CARTESIAN_POINT('',(-6.60014603862878,-10.0218796774244,-1.5));
#8640=CARTESIAN_POINT('Origin',(0.,0.,-1.5));
#8641=CARTESIAN_POINT('',(-6.60014603862878,-10.0218796774244,5.));
#8642=CARTESIAN_POINT('Origin',(0.,0.,5.));
#8643=CARTESIAN_POINT('',(5.37912937500617,10.726833976852,-1.5));
#8644=CARTESIAN_POINT('',(5.37912937500617,10.726833976852,5.));
#8645=CARTESIAN_POINT('',(-5.37912937500617,10.726833976852,-1.5));
#8646=CARTESIAN_POINT('Origin',(0.,0.,-1.5));
#8647=CARTESIAN_POINT('',(-5.37912937500617,10.726833976852,5.));
#8648=CARTESIAN_POINT('Origin',(0.,0.,5.));
#8649=CARTESIAN_POINT('',(-6.06863042059311,-5.89037560471066,5.));
#8650=CARTESIAN_POINT('Ctrl Pts',(-6.06863042059311,-5.89037560471066,5.));
#8651=CARTESIAN_POINT('Ctrl Pts',(-6.18294115692138,-6.00132867417749,5.));
#8652=CARTESIAN_POINT('Ctrl Pts',(-6.25574916854265,-6.14973629251005,5.));
#8653=CARTESIAN_POINT('Ctrl Pts',(-6.34958522348951,-6.33256064405531,5.));
#8654=CARTESIAN_POINT('Ctrl Pts',(-6.42989690394213,-6.49149718347625,5.));
#8655=CARTESIAN_POINT('Ctrl Pts',(-6.57404148726985,-6.92443841216413,5.));
#8656=CARTESIAN_POINT('Ctrl Pts',(-6.67668490053576,-7.26884512749233,5.));
#8657=CARTESIAN_POINT('Ctrl Pts',(-6.80496270259299,-8.4372608114701,5.));
#8658=CARTESIAN_POINT('Ctrl Pts',(-6.77273909127515,-9.1969740069116,5.));
#8659=CARTESIAN_POINT('Ctrl Pts',(-6.60014603862878,-10.0218796774244,5.));
#8660=CARTESIAN_POINT('',(-4.62971553586298,-4.49372618847532,5.));
#8661=CARTESIAN_POINT('',(-4.62971553586298,-4.49372618847532,5.));
#8662=CARTESIAN_POINT('',(-4.51042861629926,-3.19779215979849,5.));
#8663=CARTESIAN_POINT('Origin',(-5.32620517920381,-3.77615934370128,5.));
#8664=CARTESIAN_POINT('',(-5.02458355455784,-2.3072496837722,5.));
#8665=CARTESIAN_POINT('Origin',(0.,0.,5.));
#8666=CARTESIAN_POINT('',(-6.20653880480254,-1.76258817211517,5.));
#8667=CARTESIAN_POINT('Origin',(-5.93335250998519,-2.72454931910811,5.));
#8668=CARTESIAN_POINT('',(-8.13553012180811,-2.31040030805734,5.));
#8669=CARTESIAN_POINT('',(-8.13553012180811,-2.31040030805734,5.));
#8670=CARTESIAN_POINT('Ctrl Pts',(-11.9792754136349,-0.704954299427526,
5.));
#8671=CARTESIAN_POINT('Ctrl Pts',(-11.5957187865582,-1.04810301200968,5.));
#8672=CARTESIAN_POINT('Ctrl Pts',(-11.1804727745354,-1.35730649168446,5.));
#8673=CARTESIAN_POINT('Ctrl Pts',(-10.1618489906271,-1.95221245619236,5.));
#8674=CARTESIAN_POINT('Ctrl Pts',(-9.70098587325195,-2.10951926095094,5.));
#8675=CARTESIAN_POINT('Ctrl Pts',(-8.94253026840227,-2.32740085079442,5.));
#8676=CARTESIAN_POINT('Ctrl Pts',(-8.60665429330284,-2.34186126624272,5.));
#8677=CARTESIAN_POINT('Ctrl Pts',(-8.28801320409324,-2.3379034137458,5.));
#8678=CARTESIAN_POINT('Ctrl Pts',(-8.21242123795409,-2.33223653209814,5.));
#8679=CARTESIAN_POINT('Ctrl Pts',(-8.13553012180811,-2.31040030805734,5.));
#8680=CARTESIAN_POINT('',(-2.066899701215,8.20077591276801,5.));
#8681=CARTESIAN_POINT('Ctrl Pts',(-2.066899701215,8.20077591276801,5.));
#8682=CARTESIAN_POINT('Ctrl Pts',(-2.10583250983699,8.35524844908701,5.));
#8683=CARTESIAN_POINT('Ctrl Pts',(-2.19795327161749,8.49250584591636,5.));
#8684=CARTESIAN_POINT('Ctrl Pts',(-2.30936577700739,8.66518242905562,5.));
#8685=CARTESIAN_POINT('Ctrl Pts',(-2.40685301751263,8.81420265426477,5.));
#8686=CARTESIAN_POINT('Ctrl Pts',(-2.70971882823706,9.1555061395873,5.));
#8687=CARTESIAN_POINT('Ctrl Pts',(-2.9566620863145,9.4166013006736,5.));
#8688=CARTESIAN_POINT('Ctrl Pts',(-3.90440084957731,10.111900977829,5.));
#8689=CARTESIAN_POINT('Ctrl Pts',(-4.57844358199661,10.4638511096066,5.));
#8690=CARTESIAN_POINT('Ctrl Pts',(-5.37912937500617,10.726833976852,5.));
#8691=CARTESIAN_POINT('',(-1.57682326893955,6.25631436059049,5.));
#8692=CARTESIAN_POINT('',(-1.57682326893955,6.25631436059049,5.));
#8693=CARTESIAN_POINT('',(-0.514154938258575,5.5050418435707,5.));
#8694=CARTESIAN_POINT('Origin',(-0.607147330781379,6.50070866280939,5.));
#8695=CARTESIAN_POINT('',(0.514154938258576,5.5050418435707,5.));
#8696=CARTESIAN_POINT('Origin',(0.,0.,5.));
#8697=CARTESIAN_POINT('',(1.57682326893955,6.25631436059049,5.));
#8698=CARTESIAN_POINT('Origin',(0.60714733078138,6.50070866280939,5.));
#8699=CARTESIAN_POINT('',(2.066899701215,8.20077591276801,5.));
#8700=CARTESIAN_POINT('',(2.066899701215,8.20077591276801,5.));
#8701=CARTESIAN_POINT('Ctrl Pts',(5.37912937500617,10.726833976852,5.));
#8702=CARTESIAN_POINT('Ctrl Pts',(4.89017555917646,10.5662385503313,5.));
#8703=CARTESIAN_POINT('Ctrl Pts',(4.41477448478803,10.3612266949343,5.));
#8704=CARTESIAN_POINT('Ctrl Pts',(3.39025891472665,9.77652560343359,5.));
#8705=CARTESIAN_POINT('Ctrl Pts',(3.02359566700368,9.45605983859608,5.));
#8706=CARTESIAN_POINT('Ctrl Pts',(2.4556768726076,8.90815881192699,5.));
#8707=CARTESIAN_POINT('Ctrl Pts',(2.27521579794331,8.62451189270667,5.));
#8708=CARTESIAN_POINT('Ctrl Pts',(2.11932285414767,8.34658168851712,5.));
#8709=CARTESIAN_POINT('Ctrl Pts',(2.08643453454576,8.27828368469551,5.));
#8710=CARTESIAN_POINT('Ctrl Pts',(2.066899701215,8.20077591276801,5.));
#8711=CARTESIAN_POINT('',(8.13553012180811,-2.31040030805735,5.));
#8712=CARTESIAN_POINT('Ctrl Pts',(8.13553012180811,-2.31040030805735,5.));
#8713=CARTESIAN_POINT('Ctrl Pts',(8.28877366675838,-2.35391977490952,5.));
#8714=CARTESIAN_POINT('Ctrl Pts',(8.45370244016016,-2.34276955340631,5.));
#8715=CARTESIAN_POINT('Ctrl Pts',(8.65895100049858,-2.33262178500872,5.));
#8716=CARTESIAN_POINT('Ctrl Pts',(8.83674992145612,-2.32270547079077,5.));
#8717=CARTESIAN_POINT('Ctrl Pts',(9.28376031551307,-2.23106772742579,5.));
#8718=CARTESIAN_POINT('Ctrl Pts',(9.63334698685416,-2.14775617318037,5.));
#8719=CARTESIAN_POINT('Ctrl Pts',(10.70936355228,-1.67464016656206,5.));
#8720=CARTESIAN_POINT('Ctrl Pts',(11.3511826734672,-1.26687710288273,5.));
#8721=CARTESIAN_POINT('Ctrl Pts',(11.9792754136349,-0.704954299427529,5.));
#8722=CARTESIAN_POINT('',(6.20653880480254,-1.76258817211517,5.));
#8723=CARTESIAN_POINT('',(6.20653880480254,-1.76258817211517,5.));
#8724=CARTESIAN_POINT('',(5.02458355455784,-2.3072496837722,5.));
#8725=CARTESIAN_POINT('Origin',(5.93335250998519,-2.72454931910811,5.));
#8726=CARTESIAN_POINT('',(4.51042861629926,-3.1977921597985,5.));
#8727=CARTESIAN_POINT('Origin',(0.,0.,5.));
#8728=CARTESIAN_POINT('',(4.62971553586298,-4.49372618847532,5.));
#8729=CARTESIAN_POINT('Origin',(5.32620517920381,-3.77615934370129,5.));
#8730=CARTESIAN_POINT('',(6.06863042059311,-5.89037560471067,5.));
#8731=CARTESIAN_POINT('',(6.06863042059311,-5.89037560471067,5.));
#8732=CARTESIAN_POINT('Ctrl Pts',(6.60014603862877,-10.0218796774244,5.));
#8733=CARTESIAN_POINT('Ctrl Pts',(6.70554322747048,-9.51813553825663,5.));
#8734=CARTESIAN_POINT('Ctrl Pts',(6.76569828978878,-9.00392020319332,5.));
#8735=CARTESIAN_POINT('Ctrl Pts',(6.77159007595975,-7.82431314719937,5.));
#8736=CARTESIAN_POINT('Ctrl Pts',(6.67739020636713,-7.34654057745018,5.));
#8737=CARTESIAN_POINT('Ctrl Pts',(6.48685339577297,-6.58075796113559,5.));
#8738=CARTESIAN_POINT('Ctrl Pts',(6.33143849535284,-6.28265062646335,5.));
#8739=CARTESIAN_POINT('Ctrl Pts',(6.16869034994494,-6.00867827477288,5.));
#8740=CARTESIAN_POINT('Ctrl Pts',(6.12598670340806,-5.94604715259793,5.));
#8741=CARTESIAN_POINT('Ctrl Pts',(6.06863042059311,-5.89037560471067,5.));
#8742=CARTESIAN_POINT('Origin',(0.,0.,6.));
#8743=CARTESIAN_POINT('',(7.,-8.57252759403147E-16,12.));
#8744=CARTESIAN_POINT('Origin',(0.,0.,12.));
#8745=CARTESIAN_POINT('',(7.,-8.57252759403147E-16,6.));
#8746=CARTESIAN_POINT('',(7.,8.57252759403147E-16,6.));
#8747=CARTESIAN_POINT('Origin',(0.,0.,6.));
#8748=CARTESIAN_POINT('Origin',(0.,0.,12.));
#8749=CARTESIAN_POINT('Origin',(0.,0.,5.));
#8750=CARTESIAN_POINT('',(-13.5,-1.65327317884893E-15,6.));
#8751=CARTESIAN_POINT('Origin',(0.,0.,6.));
#8752=CARTESIAN_POINT('',(-13.5,-1.65327317884893E-15,5.));
#8753=CARTESIAN_POINT('Origin',(0.,0.,6.));
#8754=CARTESIAN_POINT('Origin',(0.,0.,5.));
#8755=CARTESIAN_POINT('',(-4.51042861629926,-3.19779215979849,-1.5));
#8756=CARTESIAN_POINT('',(-4.51042861629926,-3.19779215979849,5.));
#8757=CARTESIAN_POINT('',(-5.02458355455784,-2.3072496837722,-1.5));
#8758=CARTESIAN_POINT('Origin',(0.,0.,-1.5));
#8759=CARTESIAN_POINT('',(-5.02458355455784,-2.3072496837722,5.));
#8760=CARTESIAN_POINT('Origin',(-5.93335250998519,-2.72454931910811,5.));
#8761=CARTESIAN_POINT('',(-6.20653880480254,-1.76258817211517,-1.5));
#8762=CARTESIAN_POINT('Origin',(-5.93335250998519,-2.72454931910811,-1.5));
#8763=CARTESIAN_POINT('',(-6.20653880480254,-1.76258817211517,5.));
#8764=CARTESIAN_POINT('Origin',(-8.13553012180811,-2.31040030805734,5.));
#8765=CARTESIAN_POINT('',(-8.13553012180811,-2.31040030805734,-1.5));
#8766=CARTESIAN_POINT('',(-8.13553012180811,-2.31040030805734,-1.5));
#8767=CARTESIAN_POINT('',(-8.13553012180811,-2.31040030805734,5.));
#8768=CARTESIAN_POINT('Ctrl Pts',(-11.9792754136349,-0.704954299427526,
5.));
#8769=CARTESIAN_POINT('Ctrl Pts',(-11.9792754136349,-0.704954299427526,
-2.8));
#8770=CARTESIAN_POINT('Ctrl Pts',(-11.5957187865582,-1.04810301200968,5.));
#8771=CARTESIAN_POINT('Ctrl Pts',(-11.5957187865582,-1.04810301200968,-2.8));
#8772=CARTESIAN_POINT('Ctrl Pts',(-11.1804727745354,-1.35730649168446,5.));
#8773=CARTESIAN_POINT('Ctrl Pts',(-11.1804727745354,-1.35730649168446,-2.8));
#8774=CARTESIAN_POINT('Ctrl Pts',(-10.1618489906271,-1.95221245619236,5.));
#8775=CARTESIAN_POINT('Ctrl Pts',(-10.1618489906271,-1.95221245619236,-2.8));
#8776=CARTESIAN_POINT('Ctrl Pts',(-9.70098587325195,-2.10951926095094,5.));
#8777=CARTESIAN_POINT('Ctrl Pts',(-9.70098587325195,-2.10951926095094,-2.8));
#8778=CARTESIAN_POINT('Ctrl Pts',(-8.94253026840227,-2.32740085079442,5.));
#8779=CARTESIAN_POINT('Ctrl Pts',(-8.94253026840227,-2.32740085079442,-2.8));
#8780=CARTESIAN_POINT('Ctrl Pts',(-8.60665429330284,-2.34186126624272,5.));
#8781=CARTESIAN_POINT('Ctrl Pts',(-8.60665429330284,-2.34186126624272,-2.8));
#8782=CARTESIAN_POINT('Ctrl Pts',(-8.28801320409324,-2.3379034137458,5.));
#8783=CARTESIAN_POINT('Ctrl Pts',(-8.28801320409324,-2.3379034137458,-2.8));
#8784=CARTESIAN_POINT('Ctrl Pts',(-8.21242123795409,-2.33223653209814,5.));
#8785=CARTESIAN_POINT('Ctrl Pts',(-8.21242123795409,-2.33223653209814,-2.8));
#8786=CARTESIAN_POINT('Ctrl Pts',(-8.13553012180811,-2.31040030805734,5.));
#8787=CARTESIAN_POINT('Ctrl Pts',(-8.13553012180811,-2.31040030805734,-2.8));
#8788=CARTESIAN_POINT('Ctrl Pts',(-11.9792754136349,-0.704954299427526,
-1.5));
#8789=CARTESIAN_POINT('Ctrl Pts',(-11.5957187865582,-1.04810301200968,-1.5));
#8790=CARTESIAN_POINT('Ctrl Pts',(-11.1804727745354,-1.35730649168446,-1.5));
#8791=CARTESIAN_POINT('Ctrl Pts',(-10.1618489906271,-1.95221245619236,-1.5));
#8792=CARTESIAN_POINT('Ctrl Pts',(-9.70098587325195,-2.10951926095094,-1.5));
#8793=CARTESIAN_POINT('Ctrl Pts',(-8.94253026840227,-2.32740085079442,-1.5));
#8794=CARTESIAN_POINT('Ctrl Pts',(-8.60665429330284,-2.34186126624272,-1.5));
#8795=CARTESIAN_POINT('Ctrl Pts',(-8.28801320409324,-2.3379034137458,-1.5));
#8796=CARTESIAN_POINT('Ctrl Pts',(-8.21242123795409,-2.33223653209814,-1.5));
#8797=CARTESIAN_POINT('Ctrl Pts',(-8.13553012180811,-2.31040030805734,-1.5));
#8798=CARTESIAN_POINT('Ctrl Pts',(-6.06863042059311,-5.89037560471066,5.));
#8799=CARTESIAN_POINT('Ctrl Pts',(-6.06863042059311,-5.89037560471066,-2.8));
#8800=CARTESIAN_POINT('Ctrl Pts',(-6.18294115692138,-6.00132867417749,5.));
#8801=CARTESIAN_POINT('Ctrl Pts',(-6.18294115692138,-6.00132867417749,-2.8));
#8802=CARTESIAN_POINT('Ctrl Pts',(-6.25574916854265,-6.14973629251005,5.));
#8803=CARTESIAN_POINT('Ctrl Pts',(-6.25574916854265,-6.14973629251005,-2.8));
#8804=CARTESIAN_POINT('Ctrl Pts',(-6.34958522348951,-6.33256064405531,5.));
#8805=CARTESIAN_POINT('Ctrl Pts',(-6.34958522348951,-6.33256064405531,-2.8));
#8806=CARTESIAN_POINT('Ctrl Pts',(-6.42989690394213,-6.49149718347625,5.));
#8807=CARTESIAN_POINT('Ctrl Pts',(-6.42989690394213,-6.49149718347625,-2.8));
#8808=CARTESIAN_POINT('Ctrl Pts',(-6.57404148726985,-6.92443841216413,5.));
#8809=CARTESIAN_POINT('Ctrl Pts',(-6.57404148726985,-6.92443841216413,-2.8));
#8810=CARTESIAN_POINT('Ctrl Pts',(-6.67668490053576,-7.26884512749233,5.));
#8811=CARTESIAN_POINT('Ctrl Pts',(-6.67668490053576,-7.26884512749233,-2.8));
#8812=CARTESIAN_POINT('Ctrl Pts',(-6.80496270259299,-8.4372608114701,5.));
#8813=CARTESIAN_POINT('Ctrl Pts',(-6.80496270259299,-8.4372608114701,-2.8));
#8814=CARTESIAN_POINT('Ctrl Pts',(-6.77273909127515,-9.1969740069116,5.));
#8815=CARTESIAN_POINT('Ctrl Pts',(-6.77273909127515,-9.1969740069116,-2.8));
#8816=CARTESIAN_POINT('Ctrl Pts',(-6.60014603862878,-10.0218796774244,5.));
#8817=CARTESIAN_POINT('Ctrl Pts',(-6.60014603862878,-10.0218796774244,-2.8));
#8818=CARTESIAN_POINT('',(-6.06863042059311,-5.89037560471066,-1.5));
#8819=CARTESIAN_POINT('Ctrl Pts',(-6.06863042059311,-5.89037560471066,-1.5));
#8820=CARTESIAN_POINT('Ctrl Pts',(-6.18294115692138,-6.00132867417749,-1.5));
#8821=CARTESIAN_POINT('Ctrl Pts',(-6.25574916854265,-6.14973629251005,-1.5));
#8822=CARTESIAN_POINT('Ctrl Pts',(-6.34958522348951,-6.33256064405531,-1.5));
#8823=CARTESIAN_POINT('Ctrl Pts',(-6.42989690394213,-6.49149718347625,-1.5));
#8824=CARTESIAN_POINT('Ctrl Pts',(-6.57404148726985,-6.92443841216413,-1.5));
#8825=CARTESIAN_POINT('Ctrl Pts',(-6.67668490053576,-7.26884512749233,-1.5));
#8826=CARTESIAN_POINT('Ctrl Pts',(-6.80496270259299,-8.4372608114701,-1.5));
#8827=CARTESIAN_POINT('Ctrl Pts',(-6.77273909127515,-9.1969740069116,-1.5));
#8828=CARTESIAN_POINT('Ctrl Pts',(-6.60014603862878,-10.0218796774244,-1.5));
#8829=CARTESIAN_POINT('',(-6.06863042059311,-5.89037560471066,5.));
#8830=CARTESIAN_POINT('Origin',(-4.62971553586298,-4.49372618847532,5.));
#8831=CARTESIAN_POINT('',(-4.62971553586298,-4.49372618847532,-1.5));
#8832=CARTESIAN_POINT('',(-4.62971553586298,-4.49372618847532,-1.5));
#8833=CARTESIAN_POINT('',(-4.62971553586298,-4.49372618847532,5.));
#8834=CARTESIAN_POINT('Origin',(-5.32620517920381,-3.77615934370128,5.));
#8835=CARTESIAN_POINT('Origin',(-5.32620517920381,-3.77615934370128,-1.5));
#8836=CARTESIAN_POINT('Origin',(-8.15362319838813,-5.36431270931319,-1.5));
#8837=CARTESIAN_POINT('Origin',(0.,0.,5.));
#8838=CARTESIAN_POINT('',(-0.514154938258575,5.5050418435707,-1.5));
#8839=CARTESIAN_POINT('',(-0.514154938258575,5.5050418435707,5.));
#8840=CARTESIAN_POINT('',(0.514154938258576,5.5050418435707,-1.5));
#8841=CARTESIAN_POINT('Origin',(0.,0.,-1.5));
#8842=CARTESIAN_POINT('',(0.514154938258576,5.5050418435707,5.));
#8843=CARTESIAN_POINT('Origin',(0.60714733078138,6.50070866280939,5.));
#8844=CARTESIAN_POINT('',(1.57682326893956,6.25631436059049,-1.5));
#8845=CARTESIAN_POINT('Origin',(0.60714733078138,6.50070866280939,-1.5));
#8846=CARTESIAN_POINT('',(1.57682326893955,6.25631436059049,5.));
#8847=CARTESIAN_POINT('Origin',(2.066899701215,8.20077591276801,5.));
#8848=CARTESIAN_POINT('',(2.066899701215,8.20077591276801,-1.5));
#8849=CARTESIAN_POINT('',(2.066899701215,8.20077591276801,-1.5));
#8850=CARTESIAN_POINT('',(2.066899701215,8.20077591276801,5.));
#8851=CARTESIAN_POINT('Ctrl Pts',(5.37912937500617,10.726833976852,5.));
#8852=CARTESIAN_POINT('Ctrl Pts',(5.37912937500617,10.726833976852,-2.8));
#8853=CARTESIAN_POINT('Ctrl Pts',(4.89017555917646,10.5662385503313,5.));
#8854=CARTESIAN_POINT('Ctrl Pts',(4.89017555917646,10.5662385503313,-2.8));
#8855=CARTESIAN_POINT('Ctrl Pts',(4.41477448478803,10.3612266949343,5.));
#8856=CARTESIAN_POINT('Ctrl Pts',(4.41477448478803,10.3612266949343,-2.8));
#8857=CARTESIAN_POINT('Ctrl Pts',(3.39025891472665,9.77652560343359,5.));
#8858=CARTESIAN_POINT('Ctrl Pts',(3.39025891472665,9.77652560343359,-2.8));
#8859=CARTESIAN_POINT('Ctrl Pts',(3.02359566700368,9.45605983859608,5.));
#8860=CARTESIAN_POINT('Ctrl Pts',(3.02359566700368,9.45605983859608,-2.8));
#8861=CARTESIAN_POINT('Ctrl Pts',(2.4556768726076,8.90815881192699,5.));
#8862=CARTESIAN_POINT('Ctrl Pts',(2.4556768726076,8.90815881192699,-2.8));
#8863=CARTESIAN_POINT('Ctrl Pts',(2.27521579794331,8.62451189270667,5.));
#8864=CARTESIAN_POINT('Ctrl Pts',(2.27521579794331,8.62451189270667,-2.8));
#8865=CARTESIAN_POINT('Ctrl Pts',(2.11932285414767,8.34658168851712,5.));
#8866=CARTESIAN_POINT('Ctrl Pts',(2.11932285414767,8.34658168851712,-2.8));
#8867=CARTESIAN_POINT('Ctrl Pts',(2.08643453454576,8.27828368469551,5.));
#8868=CARTESIAN_POINT('Ctrl Pts',(2.08643453454576,8.27828368469551,-2.8));
#8869=CARTESIAN_POINT('Ctrl Pts',(2.066899701215,8.20077591276801,5.));
#8870=CARTESIAN_POINT('Ctrl Pts',(2.066899701215,8.20077591276801,-2.8));
#8871=CARTESIAN_POINT('Ctrl Pts',(5.37912937500617,10.726833976852,-1.5));
#8872=CARTESIAN_POINT('Ctrl Pts',(4.89017555917646,10.5662385503313,-1.5));
#8873=CARTESIAN_POINT('Ctrl Pts',(4.41477448478803,10.3612266949343,-1.5));
#8874=CARTESIAN_POINT('Ctrl Pts',(3.39025891472665,9.77652560343359,-1.5));
#8875=CARTESIAN_POINT('Ctrl Pts',(3.02359566700368,9.45605983859608,-1.5));
#8876=CARTESIAN_POINT('Ctrl Pts',(2.4556768726076,8.90815881192699,-1.5));
#8877=CARTESIAN_POINT('Ctrl Pts',(2.27521579794331,8.62451189270667,-1.5));
#8878=CARTESIAN_POINT('Ctrl Pts',(2.11932285414767,8.34658168851712,-1.5));
#8879=CARTESIAN_POINT('Ctrl Pts',(2.08643453454576,8.27828368469551,-1.5));
#8880=CARTESIAN_POINT('Ctrl Pts',(2.066899701215,8.20077591276801,-1.5));
#8881=CARTESIAN_POINT('Ctrl Pts',(-2.066899701215,8.20077591276801,5.));
#8882=CARTESIAN_POINT('Ctrl Pts',(-2.066899701215,8.20077591276801,-2.8));
#8883=CARTESIAN_POINT('Ctrl Pts',(-2.10583250983699,8.35524844908701,5.));
#8884=CARTESIAN_POINT('Ctrl Pts',(-2.10583250983699,8.35524844908701,-2.8));
#8885=CARTESIAN_POINT('Ctrl Pts',(-2.19795327161749,8.49250584591636,5.));
#8886=CARTESIAN_POINT('Ctrl Pts',(-2.19795327161749,8.49250584591636,-2.8));
#8887=CARTESIAN_POINT('Ctrl Pts',(-2.30936577700739,8.66518242905562,5.));
#8888=CARTESIAN_POINT('Ctrl Pts',(-2.30936577700739,8.66518242905562,-2.8));
#8889=CARTESIAN_POINT('Ctrl Pts',(-2.40685301751263,8.81420265426477,5.));
#8890=CARTESIAN_POINT('Ctrl Pts',(-2.40685301751263,8.81420265426477,-2.8));
#8891=CARTESIAN_POINT('Ctrl Pts',(-2.70971882823706,9.1555061395873,5.));
#8892=CARTESIAN_POINT('Ctrl Pts',(-2.70971882823706,9.1555061395873,-2.8));
#8893=CARTESIAN_POINT('Ctrl Pts',(-2.9566620863145,9.4166013006736,5.));
#8894=CARTESIAN_POINT('Ctrl Pts',(-2.9566620863145,9.4166013006736,-2.8));
#8895=CARTESIAN_POINT('Ctrl Pts',(-3.90440084957731,10.111900977829,5.));
#8896=CARTESIAN_POINT('Ctrl Pts',(-3.90440084957731,10.111900977829,-2.8));
#8897=CARTESIAN_POINT('Ctrl Pts',(-4.57844358199661,10.4638511096066,5.));
#8898=CARTESIAN_POINT('Ctrl Pts',(-4.57844358199661,10.4638511096066,-2.8));
#8899=CARTESIAN_POINT('Ctrl Pts',(-5.37912937500617,10.726833976852,5.));
#8900=CARTESIAN_POINT('Ctrl Pts',(-5.37912937500617,10.726833976852,-2.8));
#8901=CARTESIAN_POINT('',(-2.066899701215,8.20077591276801,-1.5));
#8902=CARTESIAN_POINT('Ctrl Pts',(-2.066899701215,8.20077591276801,-1.5));
#8903=CARTESIAN_POINT('Ctrl Pts',(-2.10583250983699,8.35524844908701,-1.5));
#8904=CARTESIAN_POINT('Ctrl Pts',(-2.19795327161749,8.49250584591636,-1.5));
#8905=CARTESIAN_POINT('Ctrl Pts',(-2.30936577700739,8.66518242905562,-1.5));
#8906=CARTESIAN_POINT('Ctrl Pts',(-2.40685301751263,8.81420265426477,-1.5));
#8907=CARTESIAN_POINT('Ctrl Pts',(-2.70971882823706,9.1555061395873,-1.5));
#8908=CARTESIAN_POINT('Ctrl Pts',(-2.9566620863145,9.4166013006736,-1.5));
#8909=CARTESIAN_POINT('Ctrl Pts',(-3.90440084957731,10.111900977829,-1.5));
#8910=CARTESIAN_POINT('Ctrl Pts',(-4.57844358199661,10.4638511096066,-1.5));
#8911=CARTESIAN_POINT('Ctrl Pts',(-5.37912937500617,10.726833976852,-1.5));
#8912=CARTESIAN_POINT('',(-2.066899701215,8.20077591276801,5.));
#8913=CARTESIAN_POINT('Origin',(-1.57682326893955,6.25631436059049,5.));
#8914=CARTESIAN_POINT('',(-1.57682326893955,6.25631436059049,-1.5));
#8915=CARTESIAN_POINT('',(-1.57682326893955,6.25631436059049,-1.5));
#8916=CARTESIAN_POINT('',(-1.57682326893955,6.25631436059049,5.));
#8917=CARTESIAN_POINT('Origin',(-0.607147330781379,6.50070866280939,5.));
#8918=CARTESIAN_POINT('Origin',(-0.607147330781379,6.50070866280939,-1.5));
#8919=CARTESIAN_POINT('Origin',(-0.000895720887666984,8.7503543314047,-1.5));
#8920=CARTESIAN_POINT('Origin',(0.,0.,5.));
#8921=CARTESIAN_POINT('',(5.02458355455784,-2.3072496837722,-1.5));
#8922=CARTESIAN_POINT('',(5.02458355455784,-2.3072496837722,5.));
#8923=CARTESIAN_POINT('',(4.51042861629926,-3.1977921597985,-1.5));
#8924=CARTESIAN_POINT('Origin',(0.,0.,-1.5));
#8925=CARTESIAN_POINT('',(4.51042861629926,-3.1977921597985,5.));
#8926=CARTESIAN_POINT('Origin',(5.32620517920381,-3.77615934370129,5.));
#8927=CARTESIAN_POINT('',(4.62971553586298,-4.49372618847532,-1.5));
#8928=CARTESIAN_POINT('Origin',(5.32620517920381,-3.77615934370129,-1.5));
#8929=CARTESIAN_POINT('',(4.62971553586298,-4.49372618847532,5.));
#8930=CARTESIAN_POINT('Origin',(6.06863042059311,-5.89037560471067,5.));
#8931=CARTESIAN_POINT('',(6.06863042059311,-5.89037560471067,-1.5));
#8932=CARTESIAN_POINT('',(6.06863042059311,-5.89037560471067,-1.5));
#8933=CARTESIAN_POINT('',(6.06863042059311,-5.89037560471067,5.));
#8934=CARTESIAN_POINT('Ctrl Pts',(6.60014603862877,-10.0218796774244,5.));
#8935=CARTESIAN_POINT('Ctrl Pts',(6.60014603862877,-10.0218796774244,-2.8));
#8936=CARTESIAN_POINT('Ctrl Pts',(6.70554322747048,-9.51813553825663,5.));
#8937=CARTESIAN_POINT('Ctrl Pts',(6.70554322747048,-9.51813553825663,-2.8));
#8938=CARTESIAN_POINT('Ctrl Pts',(6.76569828978878,-9.00392020319332,5.));
#8939=CARTESIAN_POINT('Ctrl Pts',(6.76569828978878,-9.00392020319332,-2.8));
#8940=CARTESIAN_POINT('Ctrl Pts',(6.77159007595975,-7.82431314719937,5.));
#8941=CARTESIAN_POINT('Ctrl Pts',(6.77159007595975,-7.82431314719937,-2.8));
#8942=CARTESIAN_POINT('Ctrl Pts',(6.67739020636713,-7.34654057745018,5.));
#8943=CARTESIAN_POINT('Ctrl Pts',(6.67739020636713,-7.34654057745018,-2.8));
#8944=CARTESIAN_POINT('Ctrl Pts',(6.48685339577297,-6.58075796113559,5.));
#8945=CARTESIAN_POINT('Ctrl Pts',(6.48685339577297,-6.58075796113559,-2.8));
#8946=CARTESIAN_POINT('Ctrl Pts',(6.33143849535284,-6.28265062646335,5.));
#8947=CARTESIAN_POINT('Ctrl Pts',(6.33143849535284,-6.28265062646335,-2.8));
#8948=CARTESIAN_POINT('Ctrl Pts',(6.16869034994494,-6.00867827477288,5.));
#8949=CARTESIAN_POINT('Ctrl Pts',(6.16869034994494,-6.00867827477288,-2.8));
#8950=CARTESIAN_POINT('Ctrl Pts',(6.12598670340806,-5.94604715259793,5.));
#8951=CARTESIAN_POINT('Ctrl Pts',(6.12598670340806,-5.94604715259793,-2.8));
#8952=CARTESIAN_POINT('Ctrl Pts',(6.06863042059311,-5.89037560471067,5.));
#8953=CARTESIAN_POINT('Ctrl Pts',(6.06863042059311,-5.89037560471067,-2.8));
#8954=CARTESIAN_POINT('',(6.60014603862876,-10.0218796774244,-1.5));
#8955=CARTESIAN_POINT('Ctrl Pts',(6.60014603862877,-10.0218796774244,-1.5));
#8956=CARTESIAN_POINT('Ctrl Pts',(6.70554322747048,-9.51813553825663,-1.5));
#8957=CARTESIAN_POINT('Ctrl Pts',(6.76569828978878,-9.00392020319332,-1.5));
#8958=CARTESIAN_POINT('Ctrl Pts',(6.77159007595975,-7.82431314719937,-1.5));
#8959=CARTESIAN_POINT('Ctrl Pts',(6.67739020636713,-7.34654057745018,-1.5));
#8960=CARTESIAN_POINT('Ctrl Pts',(6.48685339577297,-6.58075796113559,-1.5));
#8961=CARTESIAN_POINT('Ctrl Pts',(6.33143849535284,-6.28265062646335,-1.5));
#8962=CARTESIAN_POINT('Ctrl Pts',(6.16869034994494,-6.00867827477288,-1.5));
#8963=CARTESIAN_POINT('Ctrl Pts',(6.12598670340806,-5.94604715259793,-1.5));
#8964=CARTESIAN_POINT('Ctrl Pts',(6.06863042059311,-5.89037560471067,-1.5));
#8965=CARTESIAN_POINT('',(6.60014603862876,-10.0218796774244,5.));
#8966=CARTESIAN_POINT('Origin',(0.,0.,5.));
#8967=CARTESIAN_POINT('',(11.9792754136349,-0.704954299427529,-1.5));
#8968=CARTESIAN_POINT('Origin',(0.,0.,-1.5));
#8969=CARTESIAN_POINT('',(11.9792754136349,-0.704954299427529,5.));
#8970=CARTESIAN_POINT('Ctrl Pts',(8.13553012180811,-2.31040030805735,5.));
#8971=CARTESIAN_POINT('Ctrl Pts',(8.13553012180811,-2.31040030805735,-2.8));
#8972=CARTESIAN_POINT('Ctrl Pts',(8.28877366675838,-2.35391977490952,5.));
#8973=CARTESIAN_POINT('Ctrl Pts',(8.28877366675838,-2.35391977490952,-2.8));
#8974=CARTESIAN_POINT('Ctrl Pts',(8.45370244016016,-2.34276955340631,5.));
#8975=CARTESIAN_POINT('Ctrl Pts',(8.45370244016016,-2.34276955340631,-2.8));
#8976=CARTESIAN_POINT('Ctrl Pts',(8.65895100049858,-2.33262178500872,5.));
#8977=CARTESIAN_POINT('Ctrl Pts',(8.65895100049858,-2.33262178500872,-2.8));
#8978=CARTESIAN_POINT('Ctrl Pts',(8.83674992145612,-2.32270547079077,5.));
#8979=CARTESIAN_POINT('Ctrl Pts',(8.83674992145612,-2.32270547079077,-2.8));
#8980=CARTESIAN_POINT('Ctrl Pts',(9.28376031551307,-2.23106772742579,5.));
#8981=CARTESIAN_POINT('Ctrl Pts',(9.28376031551307,-2.23106772742579,-2.8));
#8982=CARTESIAN_POINT('Ctrl Pts',(9.63334698685416,-2.14775617318037,5.));
#8983=CARTESIAN_POINT('Ctrl Pts',(9.63334698685416,-2.14775617318037,-2.8));
#8984=CARTESIAN_POINT('Ctrl Pts',(10.70936355228,-1.67464016656206,5.));
#8985=CARTESIAN_POINT('Ctrl Pts',(10.70936355228,-1.67464016656206,-2.8));
#8986=CARTESIAN_POINT('Ctrl Pts',(11.3511826734672,-1.26687710288273,5.));
#8987=CARTESIAN_POINT('Ctrl Pts',(11.3511826734672,-1.26687710288273,-2.8));
#8988=CARTESIAN_POINT('Ctrl Pts',(11.9792754136349,-0.704954299427529,5.));
#8989=CARTESIAN_POINT('Ctrl Pts',(11.9792754136349,-0.704954299427529,-2.8));
#8990=CARTESIAN_POINT('',(8.13553012180811,-2.31040030805735,-1.5));
#8991=CARTESIAN_POINT('Ctrl Pts',(8.13553012180811,-2.31040030805735,-1.5));
#8992=CARTESIAN_POINT('Ctrl Pts',(8.28877366675838,-2.35391977490952,-1.5));
#8993=CARTESIAN_POINT('Ctrl Pts',(8.45370244016016,-2.34276955340631,-1.5));
#8994=CARTESIAN_POINT('Ctrl Pts',(8.65895100049858,-2.33262178500872,-1.5));
#8995=CARTESIAN_POINT('Ctrl Pts',(8.83674992145612,-2.32270547079077,-1.5));
#8996=CARTESIAN_POINT('Ctrl Pts',(9.28376031551307,-2.23106772742579,-1.5));
#8997=CARTESIAN_POINT('Ctrl Pts',(9.63334698685416,-2.14775617318037,-1.5));
#8998=CARTESIAN_POINT('Ctrl Pts',(10.70936355228,-1.67464016656206,-1.5));
#8999=CARTESIAN_POINT('Ctrl Pts',(11.3511826734672,-1.26687710288273,-1.5));
#9000=CARTESIAN_POINT('Ctrl Pts',(11.9792754136349,-0.704954299427529,-1.5));
#9001=CARTESIAN_POINT('',(8.13553012180811,-2.31040030805735,5.));
#9002=CARTESIAN_POINT('Origin',(6.20653880480254,-1.76258817211517,5.));
#9003=CARTESIAN_POINT('',(6.20653880480254,-1.76258817211517,-1.5));
#9004=CARTESIAN_POINT('',(6.20653880480254,-1.76258817211517,-1.5));
#9005=CARTESIAN_POINT('',(6.20653880480254,-1.76258817211517,5.));
#9006=CARTESIAN_POINT('Origin',(5.93335250998519,-2.72454931910811,5.));
#9007=CARTESIAN_POINT('Origin',(5.93335250998519,-2.72454931910811,-1.5));
#9008=CARTESIAN_POINT('Origin',(8.15451891927535,-5.36252126753871,-1.5));
#9009=CARTESIAN_POINT('',(0.,0.,0.));
#9010=CARTESIAN_POINT('Origin',(0.,-6.,-9.));
#9011=CARTESIAN_POINT('',(1.,-6.,-9.));
#9012=CARTESIAN_POINT('',(-1.,-6.,-9.));
#9013=CARTESIAN_POINT('Origin',(0.,-6.,-9.));
#9014=CARTESIAN_POINT('Origin',(0.,-6.,-9.));
#9015=CARTESIAN_POINT('',(-1.,-6.92820323027551,-9.));
#9016=CARTESIAN_POINT('',(-1.,-6.,-9.));
#9017=CARTESIAN_POINT('',(1.,-6.92820323027551,-9.));
#9018=CARTESIAN_POINT('Ctrl Pts',(1.,-6.92820323027551,-9.));
#9019=CARTESIAN_POINT('Ctrl Pts',(1.,-6.92820323027551,-9.12574806852124));
#9020=CARTESIAN_POINT('Ctrl Pts',(0.974833943897391,-6.93198034025289,-9.25975855807223));
#9021=CARTESIAN_POINT('Ctrl Pts',(0.872727208600932,-6.94557411965751,-9.50608593513711));
#9022=CARTESIAN_POINT('Ctrl Pts',(0.795795807000654,-6.95518913236708,-9.61841775537244));
#9023=CARTESIAN_POINT('Ctrl Pts',(0.618419025069236,-6.97319901589886,-9.79579453730386));
#9024=CARTESIAN_POINT('Ctrl Pts',(0.506086655807109,-6.98277103675548,-9.87272693470229));
#9025=CARTESIAN_POINT('Ctrl Pts',(0.259757407800085,-6.99626622874452,-9.97483439587313));
#9026=CARTESIAN_POINT('Ctrl Pts',(0.125746268276869,-7.,-10.));
#9027=CARTESIAN_POINT('Ctrl Pts',(-0.125746268276869,-7.,-10.));
#9028=CARTESIAN_POINT('Ctrl Pts',(-0.259757407800085,-6.99626622874452,
-9.97483439587313));
#9029=CARTESIAN_POINT('Ctrl Pts',(-0.506086655807109,-6.98277103675548,
-9.87272693470229));
#9030=CARTESIAN_POINT('Ctrl Pts',(-0.618419025069236,-6.97319901589886,
-9.79579453730386));
#9031=CARTESIAN_POINT('Ctrl Pts',(-0.795795807000653,-6.95518913236708,
-9.61841775537244));
#9032=CARTESIAN_POINT('Ctrl Pts',(-0.872727208600932,-6.94557411965751,
-9.50608593513711));
#9033=CARTESIAN_POINT('Ctrl Pts',(-0.974833943897391,-6.93198034025289,
-9.25975855807223));
#9034=CARTESIAN_POINT('Ctrl Pts',(-1.,-6.92820323027551,-9.12574806852124));
#9035=CARTESIAN_POINT('Ctrl Pts',(-1.,-6.92820323027551,-9.));
#9036=CARTESIAN_POINT('Ctrl Pts',(-1.,-6.92820323027551,-9.));
#9037=CARTESIAN_POINT('Ctrl Pts',(-1.,-6.92820323027551,-8.87425193147876));
#9038=CARTESIAN_POINT('Ctrl Pts',(-0.974833943897391,-6.93198034025289,
-8.74024144192777));
#9039=CARTESIAN_POINT('Ctrl Pts',(-0.872727208600932,-6.94557411965751,
-8.49391406486289));
#9040=CARTESIAN_POINT('Ctrl Pts',(-0.795795807000653,-6.95518913236708,
-8.38158224462756));
#9041=CARTESIAN_POINT('Ctrl Pts',(-0.618419025069235,-6.97319901589886,
-8.20420546269614));
#9042=CARTESIAN_POINT('Ctrl Pts',(-0.506086655807108,-6.98277103675548,
-8.12727306529771));
#9043=CARTESIAN_POINT('Ctrl Pts',(-0.259757407800085,-6.99626622874452,
-8.02516560412687));
#9044=CARTESIAN_POINT('Ctrl Pts',(-0.125746268276869,-7.,-8.));
#9045=CARTESIAN_POINT('Ctrl Pts',(0.125746268276869,-7.,-8.));
#9046=CARTESIAN_POINT('Ctrl Pts',(0.259757407800085,-6.99626622874452,-8.02516560412687));
#9047=CARTESIAN_POINT('Ctrl Pts',(0.506086655807109,-6.98277103675548,-8.12727306529771));
#9048=CARTESIAN_POINT('Ctrl Pts',(0.618419025069235,-6.97319901589886,-8.20420546269614));
#9049=CARTESIAN_POINT('Ctrl Pts',(0.795795807000653,-6.95518913236708,-8.38158224462756));
#9050=CARTESIAN_POINT('Ctrl Pts',(0.872727208600931,-6.94557411965751,-8.49391406486289));
#9051=CARTESIAN_POINT('Ctrl Pts',(0.974833943897391,-6.93198034025289,-8.74024144192777));
#9052=CARTESIAN_POINT('Ctrl Pts',(1.,-6.92820323027551,-8.87425193147876));
#9053=CARTESIAN_POINT('Ctrl Pts',(1.,-6.92820323027551,-9.));
#9054=CARTESIAN_POINT('Origin',(0.,-6.,-10.5));
#9055=CARTESIAN_POINT('',(1.,-6.,-12.));
#9056=CARTESIAN_POINT('',(1.,-6.,-14.5));
#9057=CARTESIAN_POINT('',(-1.,-6.,-12.));
#9058=CARTESIAN_POINT('',(0.,-6.,-12.));
#9059=CARTESIAN_POINT('',(-1.,-6.,-6.5));
#9060=CARTESIAN_POINT('Origin',(0.,-6.,-10.5));
#9061=CARTESIAN_POINT('',(-1.,-6.,-6.5));
#9062=CARTESIAN_POINT('',(-1.,-6.,-6.5));
#9063=CARTESIAN_POINT('',(1.,-6.,-6.5));
#9064=CARTESIAN_POINT('Origin',(0.,-6.,-6.5));
#9065=CARTESIAN_POINT('',(1.,-6.,-14.5));
#9066=CARTESIAN_POINT('Origin',(1.,0.,-6.5));
#9067=CARTESIAN_POINT('',(1.,-4.89897948556636,-12.));
#9068=CARTESIAN_POINT('',(1.,0.,-12.));
#9069=CARTESIAN_POINT('',(1.,-4.89897948556636,-6.5));
#9070=CARTESIAN_POINT('',(1.,0.,-6.5));
#9071=CARTESIAN_POINT('',(1.,-4.89897948556636,-5.));
#9072=CARTESIAN_POINT('Origin',(0.,0.,-6.5));
#9073=CARTESIAN_POINT('',(-1.,-4.89897948556636,-6.5));
#9074=CARTESIAN_POINT('Ctrl Pts',(1.,-4.89897948556636,-6.5));
#9075=CARTESIAN_POINT('Ctrl Pts',(1.,-4.89897948556636,-6.3740682480366));
#9076=CARTESIAN_POINT('Ctrl Pts',(0.974762796248615,-4.90433876618447,-6.23998222283811));
#9077=CARTESIAN_POINT('Ctrl Pts',(0.872605417648384,-4.92354150792771,-5.99370799496995));
#9078=CARTESIAN_POINT('Ctrl Pts',(0.795703102192088,-4.93709085101933,-5.88148953981899));
#9079=CARTESIAN_POINT('Ctrl Pts',(0.618515424645094,-4.96240337638318,-5.704301862272));
#9080=CARTESIAN_POINT('Ctrl Pts',(0.506294861197626,-4.97583347151864,-5.62739565845524));
#9081=CARTESIAN_POINT('Ctrl Pts',(0.260013306081865,-4.99476188647081,-5.52523545776417));
#9082=CARTESIAN_POINT('Ctrl Pts',(0.125924695421399,-5.,-5.5));
#9083=CARTESIAN_POINT('Ctrl Pts',(-0.1259246954214,-5.,-5.5));
#9084=CARTESIAN_POINT('Ctrl Pts',(-0.260013306081865,-4.99476188647081,
-5.52523545776417));
#9085=CARTESIAN_POINT('Ctrl Pts',(-0.506294861197626,-4.97583347151864,
-5.62739565845524));
#9086=CARTESIAN_POINT('Ctrl Pts',(-0.618515424645094,-4.96240337638318,
-5.704301862272));
#9087=CARTESIAN_POINT('Ctrl Pts',(-0.795703102192089,-4.93709085101933,
-5.88148953981899));
#9088=CARTESIAN_POINT('Ctrl Pts',(-0.872605417648382,-4.92354150792771,
-5.99370799496995));
#9089=CARTESIAN_POINT('Ctrl Pts',(-0.974762796248614,-4.90433876618447,
-6.23998222283811));
#9090=CARTESIAN_POINT('Ctrl Pts',(-1.,-4.89897948556636,-6.3740682480366));
#9091=CARTESIAN_POINT('Ctrl Pts',(-1.,-4.89897948556636,-6.5));
#9092=CARTESIAN_POINT('',(-1.,0.,-6.5));
#9093=CARTESIAN_POINT('Origin',(-1.,0.,-14.5));
#9094=CARTESIAN_POINT('',(-1.,-4.89897948556636,-12.));
#9095=CARTESIAN_POINT('',(-1.,0.,-12.));
#9096=CARTESIAN_POINT('',(-1.,-4.89897948556636,-5.));
#9097=CARTESIAN_POINT('Origin',(0.,0.,-5.));
#9098=CARTESIAN_POINT('',(-2.5,4.33012701892219,-12.));
#9099=CARTESIAN_POINT('Origin',(0.,0.,-12.));
#9100=CARTESIAN_POINT('',(-2.5,4.33012701892219,-5.));
#9101=CARTESIAN_POINT('',(-2.5,4.33012701892219,-5.));
#9102=CARTESIAN_POINT('Origin',(0.,0.,-5.));
#9103=CARTESIAN_POINT('Origin',(0.,0.,-12.));
#9104=CARTESIAN_POINT('Origin',(0.,0.,-5.));
#9105=CARTESIAN_POINT('',(5.37912937500617,-10.726833976852,-5.));
#9106=CARTESIAN_POINT('',(5.37912937500617,-10.726833976852,-0.2));
#9107=CARTESIAN_POINT('',(5.37912937500617,-10.726833976852,-5.));
#9108=CARTESIAN_POINT('',(11.9792754136349,0.704954299427522,-0.2));
#9109=CARTESIAN_POINT('Origin',(0.,0.,-0.2));
#9110=CARTESIAN_POINT('',(11.9792754136349,0.704954299427527,-5.));
#9111=CARTESIAN_POINT('',(11.9792754136349,0.704954299427527,-5.));
#9112=CARTESIAN_POINT('Origin',(0.,0.,-5.));
#9113=CARTESIAN_POINT('Origin',(0.,0.,-5.));
#9114=CARTESIAN_POINT('',(-6.60014603862877,10.0218796774244,-5.));
#9115=CARTESIAN_POINT('',(-6.60014603862875,10.0218796774245,-0.2));
#9116=CARTESIAN_POINT('',(-6.60014603862877,10.0218796774244,-5.));
#9117=CARTESIAN_POINT('',(6.60014603862878,10.0218796774244,-5.));
#9118=CARTESIAN_POINT('Origin',(0.,0.,-5.));
#9119=CARTESIAN_POINT('',(6.60014603862878,10.0218796774244,-0.2));
#9120=CARTESIAN_POINT('',(6.60014603862878,10.0218796774244,-5.));
#9121=CARTESIAN_POINT('Origin',(0.,0.,-0.2));
#9122=CARTESIAN_POINT('Origin',(0.,0.,-5.));
#9123=CARTESIAN_POINT('',(-5.37912937500618,-10.726833976852,-5.));
#9124=CARTESIAN_POINT('',(-5.37912937500617,-10.726833976852,-0.2));
#9125=CARTESIAN_POINT('',(-5.37912937500618,-10.726833976852,-5.));
#9126=CARTESIAN_POINT('',(-11.9792754136349,0.704954299427533,-5.));
#9127=CARTESIAN_POINT('Origin',(0.,0.,-5.));
#9128=CARTESIAN_POINT('',(-11.9792754136349,0.704954299427533,-0.2));
#9129=CARTESIAN_POINT('',(-11.9792754136349,0.704954299427533,-5.));
#9130=CARTESIAN_POINT('Origin',(0.,0.,-0.2));
#9131=CARTESIAN_POINT('Origin',(0.,0.,-0.2));
#9132=CARTESIAN_POINT('',(-6.75,11.6913429510899,-0.2));
#9133=CARTESIAN_POINT('Origin',(0.,0.,-0.2));
#9134=CARTESIAN_POINT('Origin',(0.,0.,-0.2));
#9135=CARTESIAN_POINT('Origin',(0.,0.,-0.2));
#9136=CARTESIAN_POINT('Origin',(0.,0.,-0.2));
#9137=CARTESIAN_POINT('Origin',(0.,0.,-5.));
#9138=CARTESIAN_POINT('',(-11.9792754136349,0.704954299427533,1.5));
#9139=CARTESIAN_POINT('',(-11.9792754136349,0.704954299427533,-5.));
#9140=CARTESIAN_POINT('',(-6.60014603862877,10.0218796774244,1.5));
#9141=CARTESIAN_POINT('Origin',(0.,0.,1.5));
#9142=CARTESIAN_POINT('',(-6.60014603862877,10.0218796774244,-5.));
#9143=CARTESIAN_POINT('Origin',(0.,0.,-5.));
#9144=CARTESIAN_POINT('',(6.60014603862878,10.0218796774244,1.5));
#9145=CARTESIAN_POINT('',(6.60014603862878,10.0218796774244,-5.));
#9146=CARTESIAN_POINT('',(11.9792754136349,0.704954299427527,1.5));
#9147=CARTESIAN_POINT('Origin',(0.,0.,1.5));
#9148=CARTESIAN_POINT('',(11.9792754136349,0.704954299427527,-5.));
#9149=CARTESIAN_POINT('Origin',(0.,0.,-5.));
#9150=CARTESIAN_POINT('',(-2.06689970121501,-8.20077591276801,-5.));
#9151=CARTESIAN_POINT('Ctrl Pts',(-5.37912937500618,-10.726833976852,-5.));
#9152=CARTESIAN_POINT('Ctrl Pts',(-4.89017555905846,-10.5662385502925,-5.));
#9153=CARTESIAN_POINT('Ctrl Pts',(-4.41477448471897,-10.3612266948947,-5.));
#9154=CARTESIAN_POINT('Ctrl Pts',(-3.39025891465935,-9.77652560339542,-5.));
#9155=CARTESIAN_POINT('Ctrl Pts',(-3.02359566682149,-9.45605983842045,-5.));
#9156=CARTESIAN_POINT('Ctrl Pts',(-2.45567687261362,-8.90815881193254,-5.));
#9157=CARTESIAN_POINT('Ctrl Pts',(-2.27521579794306,-8.62451189270596,-5.));
#9158=CARTESIAN_POINT('Ctrl Pts',(-2.11932285414849,-8.34658168851868,-5.));
#9159=CARTESIAN_POINT('Ctrl Pts',(-2.0864345345459,-8.27828368469604,-5.));
#9160=CARTESIAN_POINT('Ctrl Pts',(-2.06689970121501,-8.20077591276801,-5.));
#9161=CARTESIAN_POINT('',(-1.57682326893956,-6.25631436059049,-5.));
#9162=CARTESIAN_POINT('',(-2.06689970121501,-8.20077591276801,-5.));
#9163=CARTESIAN_POINT('',(-0.51415493825858,-5.5050418435707,-5.));
#9164=CARTESIAN_POINT('Origin',(-0.607147330781382,-6.50070866280939,-5.));
#9165=CARTESIAN_POINT('',(0.514154938258578,-5.5050418435707,-5.));
#9166=CARTESIAN_POINT('Origin',(0.,0.,-5.));
#9167=CARTESIAN_POINT('',(1.57682326893955,-6.25631436059049,-5.));
#9168=CARTESIAN_POINT('Origin',(0.607147330781379,-6.50070866280939,-5.));
#9169=CARTESIAN_POINT('',(2.066899701215,-8.20077591276801,-5.));
#9170=CARTESIAN_POINT('',(1.57682326893955,-6.25631436059049,-5.));
#9171=CARTESIAN_POINT('Ctrl Pts',(2.066899701215,-8.20077591276801,-5.));
#9172=CARTESIAN_POINT('Ctrl Pts',(2.105832509837,-8.35524844908701,-5.));
#9173=CARTESIAN_POINT('Ctrl Pts',(2.19795327161749,-8.49250584591635,-5.));
#9174=CARTESIAN_POINT('Ctrl Pts',(2.30936577701074,-8.66518242906081,-5.));
#9175=CARTESIAN_POINT('Ctrl Pts',(2.40685301751416,-8.81420265426653,-5.));
#9176=CARTESIAN_POINT('Ctrl Pts',(2.70971882824218,-9.15550613959305,-5.));
#9177=CARTESIAN_POINT('Ctrl Pts',(2.95666208631803,-9.41660130067616,-5.));
#9178=CARTESIAN_POINT('Ctrl Pts',(3.90440084969946,-10.1119009779187,-5.));
#9179=CARTESIAN_POINT('Ctrl Pts',(4.57844358216429,-10.4638511096618,-5.));
#9180=CARTESIAN_POINT('Ctrl Pts',(5.37912937500617,-10.726833976852,-5.));
#9181=CARTESIAN_POINT('',(8.13553012180811,2.31040030805735,-5.));
#9182=CARTESIAN_POINT('Ctrl Pts',(11.9792754136349,0.704954299427528,-5.));
#9183=CARTESIAN_POINT('Ctrl Pts',(11.5957187866216,1.04810301195305,-5.));
#9184=CARTESIAN_POINT('Ctrl Pts',(11.1804727745766,1.35730649166136,-5.));
#9185=CARTESIAN_POINT('Ctrl Pts',(10.1618489906858,1.95221245615685,-5.));
#9186=CARTESIAN_POINT('Ctrl Pts',(9.70098587343182,2.10951926090029,-5.));
#9187=CARTESIAN_POINT('Ctrl Pts',(8.94253026837877,2.32740085079939,-5.));
#9188=CARTESIAN_POINT('Ctrl Pts',(8.60665429329664,2.34186126624275,-5.));
#9189=CARTESIAN_POINT('Ctrl Pts',(8.28801320409168,2.33790341374574,-5.));
#9190=CARTESIAN_POINT('Ctrl Pts',(8.21242123795344,2.33223653209797,-5.));
#9191=CARTESIAN_POINT('Ctrl Pts',(8.13553012180811,2.31040030805735,-5.));
#9192=CARTESIAN_POINT('',(6.20653880480254,1.76258817211517,-5.));
#9193=CARTESIAN_POINT('',(8.13553012180811,2.31040030805735,-5.));
#9194=CARTESIAN_POINT('',(5.02458355455784,2.3072496837722,-5.));
#9195=CARTESIAN_POINT('Origin',(5.93335250998519,2.72454931910811,-5.));
#9196=CARTESIAN_POINT('',(4.51042861629926,3.1977921597985,-5.));
#9197=CARTESIAN_POINT('Origin',(0.,0.,-5.));
#9198=CARTESIAN_POINT('',(4.62971553586298,4.49372618847532,-5.));
#9199=CARTESIAN_POINT('Origin',(5.32620517920381,3.77615934370128,-5.));
#9200=CARTESIAN_POINT('',(6.06863042059311,5.89037560471066,-5.));
#9201=CARTESIAN_POINT('',(4.62971553586298,4.49372618847532,-5.));
#9202=CARTESIAN_POINT('Ctrl Pts',(6.06863042059311,5.89037560471066,-5.));
#9203=CARTESIAN_POINT('Ctrl Pts',(6.18294115692139,6.00132867417748,-5.));
#9204=CARTESIAN_POINT('Ctrl Pts',(6.25574916854267,6.14973629251004,-5.));
#9205=CARTESIAN_POINT('Ctrl Pts',(6.34958522348502,6.3325606440466,-5.));
#9206=CARTESIAN_POINT('Ctrl Pts',(6.4298969039412,6.49149718347355,-5.));
#9207=CARTESIAN_POINT('Ctrl Pts',(6.57404148726847,6.92443841215994,-5.));
#9208=CARTESIAN_POINT('Ctrl Pts',(6.67668490053567,7.26884512749145,-5.));
#9209=CARTESIAN_POINT('Ctrl Pts',(6.80496270256398,8.43726081120601,-5.));
#9210=CARTESIAN_POINT('Ctrl Pts',(6.77273909133898,9.19697400660618,-5.));
#9211=CARTESIAN_POINT('Ctrl Pts',(6.60014603862878,10.0218796774244,-5.));
#9212=CARTESIAN_POINT('',(-6.06863042059311,5.89037560471066,-5.));
#9213=CARTESIAN_POINT('Ctrl Pts',(-6.60014603862877,10.0218796774244,-5.));
#9214=CARTESIAN_POINT('Ctrl Pts',(-6.70554322746249,9.51813553829505,-5.));
#9215=CARTESIAN_POINT('Ctrl Pts',(-6.76569828978797,9.00392020322571,-5.));
#9216=CARTESIAN_POINT('Ctrl Pts',(-6.77159007596056,7.82431314720816,-5.));
#9217=CARTESIAN_POINT('Ctrl Pts',(-6.67739020638207,7.34654057751468,-5.));
#9218=CARTESIAN_POINT('Ctrl Pts',(-6.48685339577862,6.58075796115043,-5.));
#9219=CARTESIAN_POINT('Ctrl Pts',(-6.33143849535641,6.28265062646931,-5.));
#9220=CARTESIAN_POINT('Ctrl Pts',(-6.16869034994484,6.0086782747727,-5.));
#9221=CARTESIAN_POINT('Ctrl Pts',(-6.12598670340816,5.94604715259802,-5.));
#9222=CARTESIAN_POINT('Ctrl Pts',(-6.06863042059311,5.89037560471066,-5.));
#9223=CARTESIAN_POINT('',(-4.62971553586298,4.49372618847532,-5.));
#9224=CARTESIAN_POINT('',(-6.06863042059311,5.89037560471066,-5.));
#9225=CARTESIAN_POINT('',(-4.51042861629926,3.1977921597985,-5.));
#9226=CARTESIAN_POINT('Origin',(-5.32620517920381,3.77615934370128,-5.));
#9227=CARTESIAN_POINT('',(-5.02458355455783,2.30724968377221,-5.));
#9228=CARTESIAN_POINT('Origin',(0.,0.,-5.));
#9229=CARTESIAN_POINT('',(-6.20653880480254,1.76258817211517,-5.));
#9230=CARTESIAN_POINT('Origin',(-5.93335250998519,2.72454931910811,-5.));
#9231=CARTESIAN_POINT('',(-8.13553012180811,2.31040030805735,-5.));
#9232=CARTESIAN_POINT('',(-6.20653880480254,1.76258817211517,-5.));
#9233=CARTESIAN_POINT('Ctrl Pts',(-8.13553012180811,2.31040030805735,-5.));
#9234=CARTESIAN_POINT('Ctrl Pts',(-8.28877366675838,2.35391977490952,-5.));
#9235=CARTESIAN_POINT('Ctrl Pts',(-8.45370244016016,2.34276955340629,-5.));
#9236=CARTESIAN_POINT('Ctrl Pts',(-8.6589510005022,2.33262178500855,-5.));
#9237=CARTESIAN_POINT('Ctrl Pts',(-8.83674992145663,2.32270547079067,-5.));
#9238=CARTESIAN_POINT('Ctrl Pts',(-9.28376031550984,2.23106772742646,-5.));
#9239=CARTESIAN_POINT('Ctrl Pts',(-9.63334698685098,2.14775617318178,-5.));
#9240=CARTESIAN_POINT('Ctrl Pts',(-10.7093635523845,1.67464016651609,-5.));
#9241=CARTESIAN_POINT('Ctrl Pts',(-11.3511826735682,1.26687710279248,-5.));
#9242=CARTESIAN_POINT('Ctrl Pts',(-11.9792754136349,0.704954299427533,-5.));
#9243=CARTESIAN_POINT('Origin',(0.,0.,-6.));
#9244=CARTESIAN_POINT('',(3.5,-6.06217782649107,-6.));
#9245=CARTESIAN_POINT('Origin',(0.,0.,-6.));
#9246=CARTESIAN_POINT('',(3.5,-6.06217782649107,-12.));
#9247=CARTESIAN_POINT('',(3.5,-6.06217782649107,-6.));
#9248=CARTESIAN_POINT('Origin',(0.,0.,-12.));
#9249=CARTESIAN_POINT('Origin',(0.,0.,-12.));
#9250=CARTESIAN_POINT('Origin',(0.,0.,-5.));
#9251=CARTESIAN_POINT('',(-6.75,11.6913429510899,-6.));
#9252=CARTESIAN_POINT('',(-6.75,11.6913429510899,-5.));
#9253=CARTESIAN_POINT('Origin',(0.,0.,-6.));
#9254=CARTESIAN_POINT('Origin',(0.,0.,-6.));
#9255=CARTESIAN_POINT('Origin',(0.,0.,-5.));
#9256=CARTESIAN_POINT('',(-4.51042861629926,3.1977921597985,1.5));
#9257=CARTESIAN_POINT('',(-4.51042861629926,3.1977921597985,-5.));
#9258=CARTESIAN_POINT('',(-5.02458355455783,2.30724968377221,1.5));
#9259=CARTESIAN_POINT('Origin',(0.,0.,1.5));
#9260=CARTESIAN_POINT('',(-5.02458355455783,2.30724968377221,-5.));
#9261=CARTESIAN_POINT('Origin',(-5.32620517920381,3.77615934370128,-5.));
#9262=CARTESIAN_POINT('',(-4.62971553586298,4.49372618847532,1.5));
#9263=CARTESIAN_POINT('',(-4.62971553586298,4.49372618847532,-5.));
#9264=CARTESIAN_POINT('Origin',(-5.32620517920381,3.77615934370128,1.5));
#9265=CARTESIAN_POINT('Origin',(-6.06863042059311,5.89037560471066,-5.));
#9266=CARTESIAN_POINT('',(-6.06863042059311,5.89037560471066,1.5));
#9267=CARTESIAN_POINT('',(-6.06863042059311,5.89037560471066,-5.));
#9268=CARTESIAN_POINT('',(-6.06863042059311,5.89037560471066,1.5));
#9269=CARTESIAN_POINT('Ctrl Pts',(-6.60014603862877,10.0218796774244,-5.));
#9270=CARTESIAN_POINT('Ctrl Pts',(-6.60014603862877,10.0218796774244,2.8));
#9271=CARTESIAN_POINT('Ctrl Pts',(-6.70554322746249,9.51813553829505,-5.));
#9272=CARTESIAN_POINT('Ctrl Pts',(-6.70554322746249,9.51813553829505,2.8));
#9273=CARTESIAN_POINT('Ctrl Pts',(-6.76569828978797,9.00392020322571,-5.));
#9274=CARTESIAN_POINT('Ctrl Pts',(-6.76569828978797,9.00392020322571,2.8));
#9275=CARTESIAN_POINT('Ctrl Pts',(-6.77159007596056,7.82431314720816,-5.));
#9276=CARTESIAN_POINT('Ctrl Pts',(-6.77159007596056,7.82431314720816,2.8));
#9277=CARTESIAN_POINT('Ctrl Pts',(-6.67739020638207,7.34654057751468,-5.));
#9278=CARTESIAN_POINT('Ctrl Pts',(-6.67739020638207,7.34654057751468,2.8));
#9279=CARTESIAN_POINT('Ctrl Pts',(-6.48685339577862,6.58075796115043,-5.));
#9280=CARTESIAN_POINT('Ctrl Pts',(-6.48685339577862,6.58075796115043,2.8));
#9281=CARTESIAN_POINT('Ctrl Pts',(-6.33143849535641,6.28265062646931,-5.));
#9282=CARTESIAN_POINT('Ctrl Pts',(-6.33143849535641,6.28265062646931,2.8));
#9283=CARTESIAN_POINT('Ctrl Pts',(-6.16869034994484,6.0086782747727,-5.));
#9284=CARTESIAN_POINT('Ctrl Pts',(-6.16869034994484,6.0086782747727,2.8));
#9285=CARTESIAN_POINT('Ctrl Pts',(-6.12598670340816,5.94604715259802,-5.));
#9286=CARTESIAN_POINT('Ctrl Pts',(-6.12598670340816,5.94604715259802,2.8));
#9287=CARTESIAN_POINT('Ctrl Pts',(-6.06863042059311,5.89037560471066,-5.));
#9288=CARTESIAN_POINT('Ctrl Pts',(-6.06863042059311,5.89037560471066,2.8));
#9289=CARTESIAN_POINT('Ctrl Pts',(-6.60014603862877,10.0218796774244,1.5));
#9290=CARTESIAN_POINT('Ctrl Pts',(-6.70554322746249,9.51813553829505,1.5));
#9291=CARTESIAN_POINT('Ctrl Pts',(-6.76569828978797,9.00392020322571,1.5));
#9292=CARTESIAN_POINT('Ctrl Pts',(-6.77159007596056,7.82431314720816,1.5));
#9293=CARTESIAN_POINT('Ctrl Pts',(-6.67739020638207,7.34654057751468,1.5));
#9294=CARTESIAN_POINT('Ctrl Pts',(-6.48685339577862,6.58075796115043,1.5));
#9295=CARTESIAN_POINT('Ctrl Pts',(-6.33143849535641,6.28265062646931,1.5));
#9296=CARTESIAN_POINT('Ctrl Pts',(-6.16869034994484,6.0086782747727,1.5));
#9297=CARTESIAN_POINT('Ctrl Pts',(-6.12598670340816,5.94604715259802,1.5));
#9298=CARTESIAN_POINT('Ctrl Pts',(-6.06863042059311,5.89037560471066,1.5));
#9299=CARTESIAN_POINT('Ctrl Pts',(-8.13553012180811,2.31040030805735,-5.));
#9300=CARTESIAN_POINT('Ctrl Pts',(-8.13553012180811,2.31040030805735,2.8));
#9301=CARTESIAN_POINT('Ctrl Pts',(-8.28877366675838,2.35391977490952,-5.));
#9302=CARTESIAN_POINT('Ctrl Pts',(-8.28877366675838,2.35391977490952,2.8));
#9303=CARTESIAN_POINT('Ctrl Pts',(-8.45370244016016,2.34276955340629,-5.));
#9304=CARTESIAN_POINT('Ctrl Pts',(-8.45370244016016,2.34276955340629,2.8));
#9305=CARTESIAN_POINT('Ctrl Pts',(-8.6589510005022,2.33262178500855,-5.));
#9306=CARTESIAN_POINT('Ctrl Pts',(-8.6589510005022,2.33262178500855,2.8));
#9307=CARTESIAN_POINT('Ctrl Pts',(-8.83674992145663,2.32270547079067,-5.));
#9308=CARTESIAN_POINT('Ctrl Pts',(-8.83674992145663,2.32270547079067,2.8));
#9309=CARTESIAN_POINT('Ctrl Pts',(-9.28376031550984,2.23106772742646,-5.));
#9310=CARTESIAN_POINT('Ctrl Pts',(-9.28376031550984,2.23106772742646,2.8));
#9311=CARTESIAN_POINT('Ctrl Pts',(-9.63334698685098,2.14775617318178,-5.));
#9312=CARTESIAN_POINT('Ctrl Pts',(-9.63334698685098,2.14775617318178,2.8));
#9313=CARTESIAN_POINT('Ctrl Pts',(-10.7093635523845,1.67464016651609,-5.));
#9314=CARTESIAN_POINT('Ctrl Pts',(-10.7093635523845,1.67464016651609,2.8));
#9315=CARTESIAN_POINT('Ctrl Pts',(-11.3511826735682,1.26687710279248,-5.));
#9316=CARTESIAN_POINT('Ctrl Pts',(-11.3511826735682,1.26687710279248,2.8));
#9317=CARTESIAN_POINT('Ctrl Pts',(-11.9792754136349,0.704954299427533,-5.));
#9318=CARTESIAN_POINT('Ctrl Pts',(-11.9792754136349,0.704954299427533,2.8));
#9319=CARTESIAN_POINT('',(-8.13553012180811,2.31040030805735,1.5));
#9320=CARTESIAN_POINT('',(-8.13553012180811,2.31040030805735,-5.));
#9321=CARTESIAN_POINT('Ctrl Pts',(-8.13553012180811,2.31040030805735,1.5));
#9322=CARTESIAN_POINT('Ctrl Pts',(-8.28877366675838,2.35391977490952,1.5));
#9323=CARTESIAN_POINT('Ctrl Pts',(-8.45370244016016,2.34276955340629,1.5));
#9324=CARTESIAN_POINT('Ctrl Pts',(-8.6589510005022,2.33262178500855,1.5));
#9325=CARTESIAN_POINT('Ctrl Pts',(-8.83674992145663,2.32270547079067,1.5));
#9326=CARTESIAN_POINT('Ctrl Pts',(-9.28376031550984,2.23106772742646,1.5));
#9327=CARTESIAN_POINT('Ctrl Pts',(-9.63334698685098,2.14775617318178,1.5));
#9328=CARTESIAN_POINT('Ctrl Pts',(-10.7093635523845,1.67464016651609,1.5));
#9329=CARTESIAN_POINT('Ctrl Pts',(-11.3511826735682,1.26687710279248,1.5));
#9330=CARTESIAN_POINT('Ctrl Pts',(-11.9792754136349,0.704954299427533,1.5));
#9331=CARTESIAN_POINT('Origin',(-6.20653880480254,1.76258817211517,-5.));
#9332=CARTESIAN_POINT('',(-6.20653880480254,1.76258817211517,1.5));
#9333=CARTESIAN_POINT('',(-6.20653880480254,1.76258817211517,-5.));
#9334=CARTESIAN_POINT('',(-6.20653880480254,1.76258817211517,1.5));
#9335=CARTESIAN_POINT('Origin',(-5.93335250998519,2.72454931910811,-5.));
#9336=CARTESIAN_POINT('Origin',(-5.93335250998519,2.72454931910811,1.5));
#9337=CARTESIAN_POINT('Origin',(-8.72244267930302,4.37908846803365,1.5));
#9338=CARTESIAN_POINT('Origin',(0.,0.,-5.));
#9339=CARTESIAN_POINT('',(5.02458355455784,2.3072496837722,1.5));
#9340=CARTESIAN_POINT('',(5.02458355455784,2.3072496837722,-5.));
#9341=CARTESIAN_POINT('',(4.51042861629926,3.1977921597985,1.5));
#9342=CARTESIAN_POINT('Origin',(0.,0.,1.5));
#9343=CARTESIAN_POINT('',(4.51042861629926,3.1977921597985,-5.));
#9344=CARTESIAN_POINT('Origin',(5.93335250998519,2.72454931910811,-5.));
#9345=CARTESIAN_POINT('',(6.20653880480254,1.76258817211517,1.5));
#9346=CARTESIAN_POINT('',(6.20653880480254,1.76258817211517,-5.));
#9347=CARTESIAN_POINT('Origin',(5.93335250998519,2.72454931910811,1.5));
#9348=CARTESIAN_POINT('Origin',(8.13553012180811,2.31040030805735,-5.));
#9349=CARTESIAN_POINT('',(8.13553012180811,2.31040030805735,1.5));
#9350=CARTESIAN_POINT('',(8.13553012180811,2.31040030805735,-5.));
#9351=CARTESIAN_POINT('',(8.13553012180811,2.31040030805735,1.5));
#9352=CARTESIAN_POINT('Ctrl Pts',(11.9792754136349,0.704954299427528,-5.));
#9353=CARTESIAN_POINT('Ctrl Pts',(11.9792754136349,0.704954299427528,2.8));
#9354=CARTESIAN_POINT('Ctrl Pts',(11.5957187866216,1.04810301195305,-5.));
#9355=CARTESIAN_POINT('Ctrl Pts',(11.5957187866216,1.04810301195305,2.8));
#9356=CARTESIAN_POINT('Ctrl Pts',(11.1804727745766,1.35730649166136,-5.));
#9357=CARTESIAN_POINT('Ctrl Pts',(11.1804727745766,1.35730649166136,2.8));
#9358=CARTESIAN_POINT('Ctrl Pts',(10.1618489906858,1.95221245615685,-5.));
#9359=CARTESIAN_POINT('Ctrl Pts',(10.1618489906858,1.95221245615685,2.8));
#9360=CARTESIAN_POINT('Ctrl Pts',(9.70098587343182,2.10951926090029,-5.));
#9361=CARTESIAN_POINT('Ctrl Pts',(9.70098587343182,2.10951926090029,2.8));
#9362=CARTESIAN_POINT('Ctrl Pts',(8.94253026837877,2.32740085079939,-5.));
#9363=CARTESIAN_POINT('Ctrl Pts',(8.94253026837877,2.32740085079939,2.8));
#9364=CARTESIAN_POINT('Ctrl Pts',(8.60665429329664,2.34186126624275,-5.));
#9365=CARTESIAN_POINT('Ctrl Pts',(8.60665429329664,2.34186126624275,2.8));
#9366=CARTESIAN_POINT('Ctrl Pts',(8.28801320409168,2.33790341374574,-5.));
#9367=CARTESIAN_POINT('Ctrl Pts',(8.28801320409168,2.33790341374574,2.8));
#9368=CARTESIAN_POINT('Ctrl Pts',(8.21242123795344,2.33223653209797,-5.));
#9369=CARTESIAN_POINT('Ctrl Pts',(8.21242123795344,2.33223653209797,2.8));
#9370=CARTESIAN_POINT('Ctrl Pts',(8.13553012180811,2.31040030805735,-5.));
#9371=CARTESIAN_POINT('Ctrl Pts',(8.13553012180811,2.31040030805735,2.8));
#9372=CARTESIAN_POINT('Ctrl Pts',(11.9792754136349,0.704954299427528,1.5));
#9373=CARTESIAN_POINT('Ctrl Pts',(11.5957187866216,1.04810301195305,1.5));
#9374=CARTESIAN_POINT('Ctrl Pts',(11.1804727745766,1.35730649166136,1.5));
#9375=CARTESIAN_POINT('Ctrl Pts',(10.1618489906858,1.95221245615685,1.5));
#9376=CARTESIAN_POINT('Ctrl Pts',(9.70098587343182,2.10951926090029,1.5));
#9377=CARTESIAN_POINT('Ctrl Pts',(8.94253026837877,2.32740085079939,1.5));
#9378=CARTESIAN_POINT('Ctrl Pts',(8.60665429329664,2.34186126624275,1.5));
#9379=CARTESIAN_POINT('Ctrl Pts',(8.28801320409168,2.33790341374574,1.5));
#9380=CARTESIAN_POINT('Ctrl Pts',(8.21242123795344,2.33223653209797,1.5));
#9381=CARTESIAN_POINT('Ctrl Pts',(8.13553012180811,2.31040030805735,1.5));
#9382=CARTESIAN_POINT('Ctrl Pts',(6.06863042059311,5.89037560471066,-5.));
#9383=CARTESIAN_POINT('Ctrl Pts',(6.06863042059311,5.89037560471066,2.8));
#9384=CARTESIAN_POINT('Ctrl Pts',(6.18294115692139,6.00132867417748,-5.));
#9385=CARTESIAN_POINT('Ctrl Pts',(6.18294115692139,6.00132867417748,2.8));
#9386=CARTESIAN_POINT('Ctrl Pts',(6.25574916854267,6.14973629251004,-5.));
#9387=CARTESIAN_POINT('Ctrl Pts',(6.25574916854267,6.14973629251004,2.8));
#9388=CARTESIAN_POINT('Ctrl Pts',(6.34958522348502,6.3325606440466,-5.));
#9389=CARTESIAN_POINT('Ctrl Pts',(6.34958522348502,6.3325606440466,2.8));
#9390=CARTESIAN_POINT('Ctrl Pts',(6.4298969039412,6.49149718347355,-5.));
#9391=CARTESIAN_POINT('Ctrl Pts',(6.4298969039412,6.49149718347355,2.8));
#9392=CARTESIAN_POINT('Ctrl Pts',(6.57404148726847,6.92443841215994,-5.));
#9393=CARTESIAN_POINT('Ctrl Pts',(6.57404148726847,6.92443841215994,2.8));
#9394=CARTESIAN_POINT('Ctrl Pts',(6.67668490053567,7.26884512749145,-5.));
#9395=CARTESIAN_POINT('Ctrl Pts',(6.67668490053567,7.26884512749145,2.8));
#9396=CARTESIAN_POINT('Ctrl Pts',(6.80496270256398,8.43726081120601,-5.));
#9397=CARTESIAN_POINT('Ctrl Pts',(6.80496270256398,8.43726081120601,2.8));
#9398=CARTESIAN_POINT('Ctrl Pts',(6.77273909133898,9.19697400660618,-5.));
#9399=CARTESIAN_POINT('Ctrl Pts',(6.77273909133898,9.19697400660618,2.8));
#9400=CARTESIAN_POINT('Ctrl Pts',(6.60014603862878,10.0218796774244,-5.));
#9401=CARTESIAN_POINT('Ctrl Pts',(6.60014603862878,10.0218796774244,2.8));
#9402=CARTESIAN_POINT('',(6.06863042059311,5.89037560471066,1.5));
#9403=CARTESIAN_POINT('',(6.06863042059311,5.89037560471066,-5.));
#9404=CARTESIAN_POINT('Ctrl Pts',(6.06863042059311,5.89037560471066,1.5));
#9405=CARTESIAN_POINT('Ctrl Pts',(6.18294115692139,6.00132867417748,1.5));
#9406=CARTESIAN_POINT('Ctrl Pts',(6.25574916854267,6.14973629251004,1.5));
#9407=CARTESIAN_POINT('Ctrl Pts',(6.34958522348502,6.3325606440466,1.5));
#9408=CARTESIAN_POINT('Ctrl Pts',(6.4298969039412,6.49149718347355,1.5));
#9409=CARTESIAN_POINT('Ctrl Pts',(6.57404148726847,6.92443841215994,1.5));
#9410=CARTESIAN_POINT('Ctrl Pts',(6.67668490053567,7.26884512749145,1.5));
#9411=CARTESIAN_POINT('Ctrl Pts',(6.80496270256398,8.43726081120601,1.5));
#9412=CARTESIAN_POINT('Ctrl Pts',(6.77273909133898,9.19697400660618,1.5));
#9413=CARTESIAN_POINT('Ctrl Pts',(6.60014603862878,10.0218796774244,1.5));
#9414=CARTESIAN_POINT('Origin',(4.62971553586298,4.49372618847532,-5.));
#9415=CARTESIAN_POINT('',(4.62971553586298,4.49372618847532,1.5));
#9416=CARTESIAN_POINT('',(4.62971553586298,4.49372618847532,-5.));
#9417=CARTESIAN_POINT('',(4.62971553586298,4.49372618847532,1.5));
#9418=CARTESIAN_POINT('Origin',(5.32620517920381,3.77615934370128,-5.));
#9419=CARTESIAN_POINT('Origin',(5.32620517920381,3.77615934370128,1.5));
#9420=CARTESIAN_POINT('Origin',(7.57758128266783,4.37595288274577,1.5));
#9421=CARTESIAN_POINT('Origin',(0.,0.,-5.));
#9422=CARTESIAN_POINT('',(-0.51415493825858,-5.5050418435707,1.5));
#9423=CARTESIAN_POINT('',(-0.51415493825858,-5.5050418435707,-5.));
#9424=CARTESIAN_POINT('',(0.514154938258578,-5.5050418435707,1.5));
#9425=CARTESIAN_POINT('Origin',(0.,0.,1.5));
#9426=CARTESIAN_POINT('',(0.514154938258578,-5.5050418435707,-5.));
#9427=CARTESIAN_POINT('Origin',(-0.607147330781382,-6.50070866280939,-5.));
#9428=CARTESIAN_POINT('',(-1.57682326893956,-6.25631436059049,1.5));
#9429=CARTESIAN_POINT('',(-1.57682326893956,-6.25631436059049,-5.));
#9430=CARTESIAN_POINT('Origin',(-0.607147330781382,-6.50070866280939,1.5));
#9431=CARTESIAN_POINT('Origin',(-2.06689970121501,-8.20077591276801,-5.));
#9432=CARTESIAN_POINT('',(-2.06689970121501,-8.20077591276801,1.5));
#9433=CARTESIAN_POINT('',(-2.06689970121501,-8.20077591276801,-5.));
#9434=CARTESIAN_POINT('',(-2.06689970121501,-8.20077591276801,1.5));
#9435=CARTESIAN_POINT('Ctrl Pts',(-5.37912937500618,-10.726833976852,-5.));
#9436=CARTESIAN_POINT('Ctrl Pts',(-5.37912937500618,-10.726833976852,2.8));
#9437=CARTESIAN_POINT('Ctrl Pts',(-4.89017555905846,-10.5662385502925,-5.));
#9438=CARTESIAN_POINT('Ctrl Pts',(-4.89017555905846,-10.5662385502925,2.8));
#9439=CARTESIAN_POINT('Ctrl Pts',(-4.41477448471897,-10.3612266948947,-5.));
#9440=CARTESIAN_POINT('Ctrl Pts',(-4.41477448471897,-10.3612266948947,2.8));
#9441=CARTESIAN_POINT('Ctrl Pts',(-3.39025891465935,-9.77652560339542,-5.));
#9442=CARTESIAN_POINT('Ctrl Pts',(-3.39025891465935,-9.77652560339542,2.8));
#9443=CARTESIAN_POINT('Ctrl Pts',(-3.02359566682149,-9.45605983842045,-5.));
#9444=CARTESIAN_POINT('Ctrl Pts',(-3.02359566682149,-9.45605983842045,2.8));
#9445=CARTESIAN_POINT('Ctrl Pts',(-2.45567687261362,-8.90815881193254,-5.));
#9446=CARTESIAN_POINT('Ctrl Pts',(-2.45567687261362,-8.90815881193254,2.8));
#9447=CARTESIAN_POINT('Ctrl Pts',(-2.27521579794306,-8.62451189270596,-5.));
#9448=CARTESIAN_POINT('Ctrl Pts',(-2.27521579794306,-8.62451189270596,2.8));
#9449=CARTESIAN_POINT('Ctrl Pts',(-2.11932285414849,-8.34658168851868,-5.));
#9450=CARTESIAN_POINT('Ctrl Pts',(-2.11932285414849,-8.34658168851868,2.8));
#9451=CARTESIAN_POINT('Ctrl Pts',(-2.0864345345459,-8.27828368469604,-5.));
#9452=CARTESIAN_POINT('Ctrl Pts',(-2.0864345345459,-8.27828368469604,2.8));
#9453=CARTESIAN_POINT('Ctrl Pts',(-2.06689970121501,-8.20077591276801,-5.));
#9454=CARTESIAN_POINT('Ctrl Pts',(-2.06689970121501,-8.20077591276801,2.8));
#9455=CARTESIAN_POINT('',(-5.37912937500618,-10.726833976852,1.5));
#9456=CARTESIAN_POINT('',(-5.37912937500618,-10.726833976852,-5.));
#9457=CARTESIAN_POINT('Ctrl Pts',(-5.37912937500618,-10.726833976852,1.5));
#9458=CARTESIAN_POINT('Ctrl Pts',(-4.89017555905846,-10.5662385502925,1.5));
#9459=CARTESIAN_POINT('Ctrl Pts',(-4.41477448471897,-10.3612266948947,1.5));
#9460=CARTESIAN_POINT('Ctrl Pts',(-3.39025891465935,-9.77652560339542,1.5));
#9461=CARTESIAN_POINT('Ctrl Pts',(-3.02359566682149,-9.45605983842045,1.5));
#9462=CARTESIAN_POINT('Ctrl Pts',(-2.45567687261362,-8.90815881193254,1.5));
#9463=CARTESIAN_POINT('Ctrl Pts',(-2.27521579794306,-8.62451189270596,1.5));
#9464=CARTESIAN_POINT('Ctrl Pts',(-2.11932285414849,-8.34658168851868,1.5));
#9465=CARTESIAN_POINT('Ctrl Pts',(-2.0864345345459,-8.27828368469604,1.5));
#9466=CARTESIAN_POINT('Ctrl Pts',(-2.06689970121501,-8.20077591276801,1.5));
#9467=CARTESIAN_POINT('Origin',(0.,0.,-5.));
#9468=CARTESIAN_POINT('',(5.37912937500617,-10.726833976852,1.5));
#9469=CARTESIAN_POINT('',(5.37912937500617,-10.726833976852,-5.));
#9470=CARTESIAN_POINT('Origin',(0.,0.,1.5));
#9471=CARTESIAN_POINT('Ctrl Pts',(2.066899701215,-8.20077591276801,-5.));
#9472=CARTESIAN_POINT('Ctrl Pts',(2.066899701215,-8.20077591276801,2.8));
#9473=CARTESIAN_POINT('Ctrl Pts',(2.105832509837,-8.35524844908701,-5.));
#9474=CARTESIAN_POINT('Ctrl Pts',(2.105832509837,-8.35524844908701,2.8));
#9475=CARTESIAN_POINT('Ctrl Pts',(2.19795327161749,-8.49250584591635,-5.));
#9476=CARTESIAN_POINT('Ctrl Pts',(2.19795327161749,-8.49250584591635,2.8));
#9477=CARTESIAN_POINT('Ctrl Pts',(2.30936577701074,-8.66518242906081,-5.));
#9478=CARTESIAN_POINT('Ctrl Pts',(2.30936577701074,-8.66518242906081,2.8));
#9479=CARTESIAN_POINT('Ctrl Pts',(2.40685301751416,-8.81420265426653,-5.));
#9480=CARTESIAN_POINT('Ctrl Pts',(2.40685301751416,-8.81420265426653,2.8));
#9481=CARTESIAN_POINT('Ctrl Pts',(2.70971882824218,-9.15550613959305,-5.));
#9482=CARTESIAN_POINT('Ctrl Pts',(2.70971882824218,-9.15550613959305,2.8));
#9483=CARTESIAN_POINT('Ctrl Pts',(2.95666208631803,-9.41660130067616,-5.));
#9484=CARTESIAN_POINT('Ctrl Pts',(2.95666208631803,-9.41660130067616,2.8));
#9485=CARTESIAN_POINT('Ctrl Pts',(3.90440084969946,-10.1119009779187,-5.));
#9486=CARTESIAN_POINT('Ctrl Pts',(3.90440084969946,-10.1119009779187,2.8));
#9487=CARTESIAN_POINT('Ctrl Pts',(4.57844358216429,-10.4638511096618,-5.));
#9488=CARTESIAN_POINT('Ctrl Pts',(4.57844358216429,-10.4638511096618,2.8));
#9489=CARTESIAN_POINT('Ctrl Pts',(5.37912937500617,-10.726833976852,-5.));
#9490=CARTESIAN_POINT('Ctrl Pts',(5.37912937500617,-10.726833976852,2.8));
#9491=CARTESIAN_POINT('',(2.066899701215,-8.20077591276801,1.5));
#9492=CARTESIAN_POINT('',(2.066899701215,-8.20077591276801,-5.));
#9493=CARTESIAN_POINT('Ctrl Pts',(2.066899701215,-8.20077591276801,1.5));
#9494=CARTESIAN_POINT('Ctrl Pts',(2.105832509837,-8.35524844908701,1.5));
#9495=CARTESIAN_POINT('Ctrl Pts',(2.19795327161749,-8.49250584591635,1.5));
#9496=CARTESIAN_POINT('Ctrl Pts',(2.30936577701074,-8.66518242906081,1.5));
#9497=CARTESIAN_POINT('Ctrl Pts',(2.40685301751416,-8.81420265426653,1.5));
#9498=CARTESIAN_POINT('Ctrl Pts',(2.70971882824218,-9.15550613959305,1.5));
#9499=CARTESIAN_POINT('Ctrl Pts',(2.95666208631803,-9.41660130067616,1.5));
#9500=CARTESIAN_POINT('Ctrl Pts',(3.90440084969946,-10.1119009779187,1.5));
#9501=CARTESIAN_POINT('Ctrl Pts',(4.57844358216429,-10.4638511096618,1.5));
#9502=CARTESIAN_POINT('Ctrl Pts',(5.37912937500617,-10.726833976852,1.5));
#9503=CARTESIAN_POINT('Origin',(1.57682326893955,-6.25631436059049,-5.));
#9504=CARTESIAN_POINT('',(1.57682326893955,-6.25631436059049,1.5));
#9505=CARTESIAN_POINT('',(1.57682326893955,-6.25631436059049,-5.));
#9506=CARTESIAN_POINT('',(1.57682326893955,-6.25631436059049,1.5));
#9507=CARTESIAN_POINT('Origin',(0.607147330781379,-6.50070866280939,-5.));
#9508=CARTESIAN_POINT('Origin',(0.607147330781379,-6.50070866280939,1.5));
#9509=CARTESIAN_POINT('Origin',(-0.566820186385169,-9.74328117350263,1.5));
#9510=CARTESIAN_POINT('',(0.,0.,0.));
#9511=CARTESIAN_POINT('Origin',(-0.57721779446269,-7.,9.01236733960726));
#9512=CARTESIAN_POINT('',(-0.57721779446269,-7.,9.01236733960726));
#9513=CARTESIAN_POINT('',(-0.277898466954226,-7.,9.50606894332475));
#9514=CARTESIAN_POINT('',(-0.502387962585574,-7.,9.13579274053664));
#9515=CARTESIAN_POINT('',(-0.57721779446269,-6.6,9.01236733960726));
#9516=CARTESIAN_POINT('',(-0.57721779446269,-7.,9.01236733960726));
#9517=CARTESIAN_POINT('',(-0.277898466954226,-6.6,9.50606894332475));
#9518=CARTESIAN_POINT('',(-0.277898466954226,-6.6,9.50606894332475));
#9519=CARTESIAN_POINT('',(-0.277898466954226,-7.,9.50606894332475));
#9520=CARTESIAN_POINT('Origin',(-0.299319327508464,-7.,8.50629839628252));
#9521=CARTESIAN_POINT('',(-0.299319327508464,-7.,8.50629839628252));
#9522=CARTESIAN_POINT('',(-0.36879394424702,-7.,8.6328156321137));
#9523=CARTESIAN_POINT('',(-0.299319327508464,-6.6,8.50629839628252));
#9524=CARTESIAN_POINT('',(-0.299319327508464,-7.,8.50629839628252));
#9525=CARTESIAN_POINT('',(-0.57721779446269,-6.6,9.01236733960726));
#9526=CARTESIAN_POINT('Origin',(0.277898466954227,-7.,8.49393105667526));
#9527=CARTESIAN_POINT('',(0.277898466954227,-7.,8.49393105667526));
#9528=CARTESIAN_POINT('',(0.133594018338554,-7.,8.49702289157707));
#9529=CARTESIAN_POINT('',(0.277898466954227,-6.6,8.49393105667526));
#9530=CARTESIAN_POINT('',(0.277898466954227,-7.,8.49393105667526));
#9531=CARTESIAN_POINT('',(-0.299319327508464,-6.6,8.50629839628252));
#9532=CARTESIAN_POINT('Origin',(0.57721779446269,-7.,8.98763266039274));
#9533=CARTESIAN_POINT('',(0.57721779446269,-7.,8.98763266039274));
#9534=CARTESIAN_POINT('',(0.502387962585574,-7.,8.86420725946337));
#9535=CARTESIAN_POINT('',(0.57721779446269,-6.6,8.98763266039274));
#9536=CARTESIAN_POINT('',(0.57721779446269,-7.,8.98763266039274));
#9537=CARTESIAN_POINT('',(0.277898466954227,-6.6,8.49393105667526));
#9538=CARTESIAN_POINT('Origin',(0.299319327508464,-7.,9.49370160371748));
#9539=CARTESIAN_POINT('',(0.299319327508464,-7.,9.49370160371748));
#9540=CARTESIAN_POINT('',(0.36879394424702,-7.,9.3671843678863));
#9541=CARTESIAN_POINT('',(0.299319327508464,-6.6,9.49370160371748));
#9542=CARTESIAN_POINT('',(0.299319327508464,-7.,9.49370160371748));
#9543=CARTESIAN_POINT('',(0.57721779446269,-6.6,8.98763266039274));
#9544=CARTESIAN_POINT('Origin',(-0.277898466954226,-7.,9.50606894332475));
#9545=CARTESIAN_POINT('',(-0.133594018338554,-7.,9.50297710842293));
#9546=CARTESIAN_POINT('',(0.299319327508464,-6.6,9.49370160371748));
#9547=CARTESIAN_POINT('Origin',(6.93889390390723E-17,-6.6,9.));
#9548=CARTESIAN_POINT('Origin',(0.,-6.,9.));
#9549=CARTESIAN_POINT('',(-1.,-7.,9.));
#9550=CARTESIAN_POINT('Origin',(0.,-7.,9.));
#9551=CARTESIAN_POINT('',(-1.,-6.,9.));
#9552=CARTESIAN_POINT('',(-1.,-6.,9.));
#9553=CARTESIAN_POINT('Origin',(0.,-6.,9.));
#9554=CARTESIAN_POINT('Origin',(0.,-7.,9.));
#9555=CARTESIAN_POINT('Origin',(0.,-6.,9.));
#9556=CARTESIAN_POINT('',(0.,0.,0.));
#9557=CARTESIAN_POINT('Origin',(-0.57721779446269,-7.,-9.01236733960726));
#9558=CARTESIAN_POINT('',(-0.57721779446269,-7.,-9.01236733960726));
#9559=CARTESIAN_POINT('',(-0.277898466954226,-7.,-9.50606894332475));
#9560=CARTESIAN_POINT('',(-0.502387962585574,-7.,-9.13579274053664));
#9561=CARTESIAN_POINT('',(-0.277898466954226,-6.6,-9.50606894332475));
#9562=CARTESIAN_POINT('',(-0.277898466954226,-7.,-9.50606894332475));
#9563=CARTESIAN_POINT('',(-0.57721779446269,-6.6,-9.01236733960726));
#9564=CARTESIAN_POINT('',(-0.277898466954226,-6.6,-9.50606894332475));
#9565=CARTESIAN_POINT('',(-0.57721779446269,-7.,-9.01236733960726));
#9566=CARTESIAN_POINT('Origin',(-0.299319327508464,-7.,-8.50629839628252));
#9567=CARTESIAN_POINT('',(-0.299319327508464,-7.,-8.50629839628252));
#9568=CARTESIAN_POINT('',(-0.36879394424702,-7.,-8.6328156321137));
#9569=CARTESIAN_POINT('',(-0.299319327508464,-6.6,-8.50629839628252));
#9570=CARTESIAN_POINT('',(-0.57721779446269,-6.6,-9.01236733960726));
#9571=CARTESIAN_POINT('',(-0.299319327508464,-7.,-8.50629839628252));
#9572=CARTESIAN_POINT('Origin',(0.277898466954227,-7.,-8.49393105667526));
#9573=CARTESIAN_POINT('',(0.277898466954227,-7.,-8.49393105667526));
#9574=CARTESIAN_POINT('',(0.133594018338554,-7.,-8.49702289157707));
#9575=CARTESIAN_POINT('',(0.277898466954227,-6.6,-8.49393105667526));
#9576=CARTESIAN_POINT('',(-0.299319327508464,-6.6,-8.50629839628252));
#9577=CARTESIAN_POINT('',(0.277898466954227,-7.,-8.49393105667526));
#9578=CARTESIAN_POINT('Origin',(0.57721779446269,-7.,-8.98763266039274));
#9579=CARTESIAN_POINT('',(0.57721779446269,-7.,-8.98763266039274));
#9580=CARTESIAN_POINT('',(0.502387962585574,-7.,-8.86420725946337));
#9581=CARTESIAN_POINT('',(0.57721779446269,-6.6,-8.98763266039274));
#9582=CARTESIAN_POINT('',(0.277898466954227,-6.6,-8.49393105667526));
#9583=CARTESIAN_POINT('',(0.57721779446269,-7.,-8.98763266039274));
#9584=CARTESIAN_POINT('Origin',(0.299319327508464,-7.,-9.49370160371748));
#9585=CARTESIAN_POINT('',(0.299319327508464,-7.,-9.49370160371748));
#9586=CARTESIAN_POINT('',(0.36879394424702,-7.,-9.3671843678863));
#9587=CARTESIAN_POINT('',(0.299319327508464,-6.6,-9.49370160371748));
#9588=CARTESIAN_POINT('',(0.57721779446269,-6.6,-8.98763266039274));
#9589=CARTESIAN_POINT('',(0.299319327508464,-7.,-9.49370160371748));
#9590=CARTESIAN_POINT('Origin',(-0.277898466954226,-7.,-9.50606894332475));
#9591=CARTESIAN_POINT('',(-0.133594018338554,-7.,-9.50297710842293));
#9592=CARTESIAN_POINT('',(0.299319327508464,-6.6,-9.49370160371748));
#9593=CARTESIAN_POINT('Origin',(6.93889390390723E-17,-6.6,-9.));
#9594=CARTESIAN_POINT('Origin',(0.,-6.,-9.));
#9595=CARTESIAN_POINT('',(-1.,-6.,-9.));
#9596=CARTESIAN_POINT('Origin',(0.,-6.,-9.));
#9597=CARTESIAN_POINT('',(-1.,-7.,-9.));
#9598=CARTESIAN_POINT('',(-1.,-6.,-9.));
#9599=CARTESIAN_POINT('Origin',(0.,-7.,-9.));
#9600=CARTESIAN_POINT('Origin',(0.,-7.,-9.));
#9601=CARTESIAN_POINT('Origin',(0.,-6.,-9.));
#9602=CARTESIAN_POINT('',(0.,0.,0.));
#9603=CARTESIAN_POINT('Origin',(1.,0.,6.5));
#9604=CARTESIAN_POINT('',(1.,-4.89897948556636,14.5));
#9605=CARTESIAN_POINT('',(1.,-4.89897948556636,6.5));
#9606=CARTESIAN_POINT('',(1.,-4.89897948556636,12.));
#9607=CARTESIAN_POINT('',(1.,-4.,14.5));
#9608=CARTESIAN_POINT('',(1.,0.,14.5));
#9609=CARTESIAN_POINT('',(1.,-4.,6.5));
#9610=CARTESIAN_POINT('',(1.,-4.,8.5));
#9611=CARTESIAN_POINT('',(1.,0.,6.5));
#9612=CARTESIAN_POINT('Origin',(0.,0.,6.5));
#9613=CARTESIAN_POINT('',(-1.,-4.89897948556636,6.5));
#9614=CARTESIAN_POINT('Ctrl Pts',(1.,-4.89897948556636,6.5));
#9615=CARTESIAN_POINT('Ctrl Pts',(1.,-4.89897948556636,6.3740682480366));
#9616=CARTESIAN_POINT('Ctrl Pts',(0.974762796248614,-4.90433876618447,6.23998222283811));
#9617=CARTESIAN_POINT('Ctrl Pts',(0.872605417648382,-4.92354150792771,5.99370799496995));
#9618=CARTESIAN_POINT('Ctrl Pts',(0.795703102192088,-4.93709085101933,5.88148953981899));
#9619=CARTESIAN_POINT('Ctrl Pts',(0.618515424645094,-4.96240337638318,5.704301862272));
#9620=CARTESIAN_POINT('Ctrl Pts',(0.506294861197626,-4.97583347151864,5.62739565845524));
#9621=CARTESIAN_POINT('Ctrl Pts',(0.260013306081865,-4.99476188647081,5.52523545776417));
#9622=CARTESIAN_POINT('Ctrl Pts',(0.125924695421399,-5.,5.5));
#9623=CARTESIAN_POINT('Ctrl Pts',(-0.1259246954214,-5.,5.5));
#9624=CARTESIAN_POINT('Ctrl Pts',(-0.260013306081865,-4.99476188647081,
5.52523545776417));
#9625=CARTESIAN_POINT('Ctrl Pts',(-0.506294861197626,-4.97583347151864,
5.62739565845524));
#9626=CARTESIAN_POINT('Ctrl Pts',(-0.618515424645094,-4.96240337638318,
5.704301862272));
#9627=CARTESIAN_POINT('Ctrl Pts',(-0.795703102192089,-4.93709085101933,
5.88148953981899));
#9628=CARTESIAN_POINT('Ctrl Pts',(-0.872605417648384,-4.92354150792771,
5.99370799496995));
#9629=CARTESIAN_POINT('Ctrl Pts',(-0.974762796248615,-4.90433876618447,
6.23998222283811));
#9630=CARTESIAN_POINT('Ctrl Pts',(-1.,-4.89897948556636,6.3740682480366));
#9631=CARTESIAN_POINT('Ctrl Pts',(-1.,-4.89897948556636,6.5));
#9632=CARTESIAN_POINT('',(-1.,-4.,6.5));
#9633=CARTESIAN_POINT('Origin',(0.,-4.,6.5));
#9634=CARTESIAN_POINT('',(-1.,0.,6.5));
#9635=CARTESIAN_POINT('Origin',(0.,-4.,10.5));
#9636=CARTESIAN_POINT('',(-1.,-4.,14.5));
#9637=CARTESIAN_POINT('Origin',(0.,-4.,14.5));
#9638=CARTESIAN_POINT('',(-1.,-4.,12.5));
#9639=CARTESIAN_POINT('Origin',(-1.,0.,14.5));
#9640=CARTESIAN_POINT('',(-1.,-4.89897948556636,14.5));
#9641=CARTESIAN_POINT('',(-1.,-4.89897948556636,12.));
#9642=CARTESIAN_POINT('',(-1.,0.,14.5));
#9643=CARTESIAN_POINT('Origin',(0.,0.,14.5));
#9644=CARTESIAN_POINT('Ctrl Pts',(-1.,-4.89897948556636,14.5));
#9645=CARTESIAN_POINT('Ctrl Pts',(-1.,-4.89897948556636,14.6259317519634));
#9646=CARTESIAN_POINT('Ctrl Pts',(-0.974762796248614,-4.90433876618447,
14.7600177771619));
#9647=CARTESIAN_POINT('Ctrl Pts',(-0.872605417648382,-4.92354150792771,
15.0062920050301));
#9648=CARTESIAN_POINT('Ctrl Pts',(-0.795703102192089,-4.93709085101933,
15.118510460181));
#9649=CARTESIAN_POINT('Ctrl Pts',(-0.618515424645094,-4.96240337638318,
15.295698137728));
#9650=CARTESIAN_POINT('Ctrl Pts',(-0.506294861197627,-4.97583347151864,
15.3726043415448));
#9651=CARTESIAN_POINT('Ctrl Pts',(-0.260013306081865,-4.99476188647081,
15.4747645422358));
#9652=CARTESIAN_POINT('Ctrl Pts',(-0.1259246954214,-5.,15.5));
#9653=CARTESIAN_POINT('Ctrl Pts',(0.125924695421399,-5.,15.5));
#9654=CARTESIAN_POINT('Ctrl Pts',(0.260013306081865,-4.99476188647081,15.4747645422358));
#9655=CARTESIAN_POINT('Ctrl Pts',(0.506294861197627,-4.97583347151864,15.3726043415448));
#9656=CARTESIAN_POINT('Ctrl Pts',(0.618515424645094,-4.96240337638318,15.295698137728));
#9657=CARTESIAN_POINT('Ctrl Pts',(0.795703102192089,-4.93709085101933,15.118510460181));
#9658=CARTESIAN_POINT('Ctrl Pts',(0.872605417648383,-4.92354150792771,15.0062920050301));
#9659=CARTESIAN_POINT('Ctrl Pts',(0.974762796248613,-4.90433876618447,14.7600177771619));
#9660=CARTESIAN_POINT('Ctrl Pts',(1.,-4.89897948556636,14.6259317519634));
#9661=CARTESIAN_POINT('Ctrl Pts',(1.,-4.89897948556636,14.5));
#9662=CARTESIAN_POINT('Origin',(0.,0.,3.5));
#9663=CARTESIAN_POINT('',(5.,6.12323399573677E-16,3.5));
#9664=CARTESIAN_POINT('Origin',(0.,0.,3.5));
#9665=CARTESIAN_POINT('Origin',(0.,0.,12.));
#9666=CARTESIAN_POINT('',(5.,6.12323399573677E-16,23.));
#9667=CARTESIAN_POINT('Origin',(0.,0.,23.));
#9668=CARTESIAN_POINT('',(5.,6.12323399573677E-16,12.));
#9669=CARTESIAN_POINT('Origin',(0.,0.,23.));
#9670=CARTESIAN_POINT('',(0.,0.,0.));
#9671=CARTESIAN_POINT('Origin',(1.,0.,-6.5));
#9672=CARTESIAN_POINT('',(1.,-4.89897948556636,-14.5));
#9673=CARTESIAN_POINT('',(1.,-4.89897948556636,-6.5));
#9674=CARTESIAN_POINT('',(1.,-4.89897948556636,-12.));
#9675=CARTESIAN_POINT('',(1.,-4.,-6.5));
#9676=CARTESIAN_POINT('',(1.,0.,-6.5));
#9677=CARTESIAN_POINT('',(1.,-4.,-14.5));
#9678=CARTESIAN_POINT('',(1.,-4.,-8.5));
#9679=CARTESIAN_POINT('',(1.,0.,-14.5));
#9680=CARTESIAN_POINT('Origin',(0.,0.,-6.5));
#9681=CARTESIAN_POINT('',(-1.,-4.89897948556636,-6.5));
#9682=CARTESIAN_POINT('Ctrl Pts',(1.,-4.89897948556636,-6.5));
#9683=CARTESIAN_POINT('Ctrl Pts',(1.,-4.89897948556636,-6.3740682480366));
#9684=CARTESIAN_POINT('Ctrl Pts',(0.974762796248615,-4.90433876618447,-6.23998222283811));
#9685=CARTESIAN_POINT('Ctrl Pts',(0.872605417648384,-4.92354150792771,-5.99370799496995));
#9686=CARTESIAN_POINT('Ctrl Pts',(0.795703102192088,-4.93709085101933,-5.88148953981899));
#9687=CARTESIAN_POINT('Ctrl Pts',(0.618515424645094,-4.96240337638318,-5.704301862272));
#9688=CARTESIAN_POINT('Ctrl Pts',(0.506294861197626,-4.97583347151864,-5.62739565845524));
#9689=CARTESIAN_POINT('Ctrl Pts',(0.260013306081865,-4.99476188647081,-5.52523545776417));
#9690=CARTESIAN_POINT('Ctrl Pts',(0.125924695421399,-5.,-5.5));
#9691=CARTESIAN_POINT('Ctrl Pts',(-0.1259246954214,-5.,-5.5));
#9692=CARTESIAN_POINT('Ctrl Pts',(-0.260013306081865,-4.99476188647081,
-5.52523545776417));
#9693=CARTESIAN_POINT('Ctrl Pts',(-0.506294861197626,-4.97583347151864,
-5.62739565845524));
#9694=CARTESIAN_POINT('Ctrl Pts',(-0.618515424645094,-4.96240337638318,
-5.704301862272));
#9695=CARTESIAN_POINT('Ctrl Pts',(-0.795703102192089,-4.93709085101933,
-5.88148953981899));
#9696=CARTESIAN_POINT('Ctrl Pts',(-0.872605417648382,-4.92354150792771,
-5.99370799496995));
#9697=CARTESIAN_POINT('Ctrl Pts',(-0.974762796248614,-4.90433876618447,
-6.23998222283811));
#9698=CARTESIAN_POINT('Ctrl Pts',(-1.,-4.89897948556636,-6.3740682480366));
#9699=CARTESIAN_POINT('Ctrl Pts',(-1.,-4.89897948556636,-6.5));
#9700=CARTESIAN_POINT('',(-1.,-4.,-6.5));
#9701=CARTESIAN_POINT('',(-1.,0.,-6.5));
#9702=CARTESIAN_POINT('Origin',(0.,-4.,-6.5));
#9703=CARTESIAN_POINT('Origin',(0.,-4.,-10.5));
#9704=CARTESIAN_POINT('',(-1.,-4.,-14.5));
#9705=CARTESIAN_POINT('',(-1.,-4.,-12.5));
#9706=CARTESIAN_POINT('Origin',(0.,-4.,-14.5));
#9707=CARTESIAN_POINT('Origin',(-1.,0.,-14.5));
#9708=CARTESIAN_POINT('',(-1.,-4.89897948556636,-14.5));
#9709=CARTESIAN_POINT('',(-1.,-4.89897948556636,-12.));
#9710=CARTESIAN_POINT('',(-1.,0.,-14.5));
#9711=CARTESIAN_POINT('Origin',(0.,0.,-14.5));
#9712=CARTESIAN_POINT('Ctrl Pts',(-1.,-4.89897948556636,-14.5));
#9713=CARTESIAN_POINT('Ctrl Pts',(-1.,-4.89897948556636,-14.6259317519634));
#9714=CARTESIAN_POINT('Ctrl Pts',(-0.974762796248615,-4.90433876618447,
-14.7600177771619));
#9715=CARTESIAN_POINT('Ctrl Pts',(-0.872605417648385,-4.92354150792771,
-15.00629200503));
#9716=CARTESIAN_POINT('Ctrl Pts',(-0.795703102192088,-4.93709085101933,
-15.118510460181));
#9717=CARTESIAN_POINT('Ctrl Pts',(-0.618515424645093,-4.96240337638318,
-15.295698137728));
#9718=CARTESIAN_POINT('Ctrl Pts',(-0.506294861197626,-4.97583347151864,
-15.3726043415448));
#9719=CARTESIAN_POINT('Ctrl Pts',(-0.260013306081865,-4.99476188647081,
-15.4747645422358));
#9720=CARTESIAN_POINT('Ctrl Pts',(-0.125924695421399,-5.,-15.5));
#9721=CARTESIAN_POINT('Ctrl Pts',(0.1259246954214,-5.,-15.5));
#9722=CARTESIAN_POINT('Ctrl Pts',(0.260013306081866,-4.99476188647081,-15.4747645422358));
#9723=CARTESIAN_POINT('Ctrl Pts',(0.506294861197627,-4.97583347151864,-15.3726043415448));
#9724=CARTESIAN_POINT('Ctrl Pts',(0.618515424645094,-4.96240337638318,-15.295698137728));
#9725=CARTESIAN_POINT('Ctrl Pts',(0.795703102192089,-4.93709085101933,-15.118510460181));
#9726=CARTESIAN_POINT('Ctrl Pts',(0.872605417648382,-4.92354150792771,-15.0062920050301));
#9727=CARTESIAN_POINT('Ctrl Pts',(0.974762796248614,-4.90433876618447,-14.7600177771619));
#9728=CARTESIAN_POINT('Ctrl Pts',(1.,-4.89897948556636,-14.6259317519634));
#9729=CARTESIAN_POINT('Ctrl Pts',(1.,-4.89897948556636,-14.5));
#9730=CARTESIAN_POINT('Origin',(0.,0.,-3.5));
#9731=CARTESIAN_POINT('',(5.,6.12323399573677E-16,-3.5));
#9732=CARTESIAN_POINT('Origin',(0.,0.,-3.5));
#9733=CARTESIAN_POINT('Origin',(0.,0.,-12.));
#9734=CARTESIAN_POINT('',(5.,6.12323399573677E-16,-23.));
#9735=CARTESIAN_POINT('',(5.,6.12323399573677E-16,-12.));
#9736=CARTESIAN_POINT('Origin',(0.,0.,-23.));
#9737=CARTESIAN_POINT('Origin',(0.,0.,-23.));
#9738=CARTESIAN_POINT('',(0.,0.,0.));
#9739=CARTESIAN_POINT('Origin',(0.,-4.,-10.5));
#9740=CARTESIAN_POINT('',(-1.,-4.,-6.5));
#9741=CARTESIAN_POINT('',(1.,-4.,-6.5));
#9742=CARTESIAN_POINT('Origin',(0.,-4.,-6.5));
#9743=CARTESIAN_POINT('',(1.,-4.,-14.5));
#9744=CARTESIAN_POINT('',(1.,-4.,-8.5));
#9745=CARTESIAN_POINT('',(-1.,-4.,-14.5));
#9746=CARTESIAN_POINT('Origin',(0.,-4.,-14.5));
#9747=CARTESIAN_POINT('',(-1.,-4.,-12.5));
#9748=CARTESIAN_POINT('Origin',(-1.,0.,-14.5));
#9749=CARTESIAN_POINT('',(-1.,-6.,-14.5));
#9750=CARTESIAN_POINT('',(-1.,0.,-14.5));
#9751=CARTESIAN_POINT('',(-1.,-6.,-6.5));
#9752=CARTESIAN_POINT('',(-1.,-6.,-6.5));
#9753=CARTESIAN_POINT('',(-1.,0.,-6.5));
#9754=CARTESIAN_POINT('Origin',(0.,0.,-6.5));
#9755=CARTESIAN_POINT('',(1.,-6.,-6.5));
#9756=CARTESIAN_POINT('Origin',(0.,-6.,-6.5));
#9757=CARTESIAN_POINT('',(1.,0.,-6.5));
#9758=CARTESIAN_POINT('Origin',(0.,0.,-14.5));
#9759=CARTESIAN_POINT('',(1.,-6.,-14.5));
#9760=CARTESIAN_POINT('',(1.,0.,-14.5));
#9761=CARTESIAN_POINT('Origin',(0.,-6.,-14.5));
#9762=CARTESIAN_POINT('Origin',(1.,0.,-6.5));
#9763=CARTESIAN_POINT('',(1.,-6.,-14.5));
#9764=CARTESIAN_POINT('Origin',(0.,-6.,-10.5));
#9765=CARTESIAN_POINT('',(0.,0.,0.));
#9766=CARTESIAN_POINT('Origin',(0.,-4.,10.5));
#9767=CARTESIAN_POINT('',(-1.,-4.,6.5));
#9768=CARTESIAN_POINT('',(1.,-4.,6.5));
#9769=CARTESIAN_POINT('Origin',(0.,-4.,6.5));
#9770=CARTESIAN_POINT('',(-1.,-4.,14.5));
#9771=CARTESIAN_POINT('',(-1.,-4.,12.5));
#9772=CARTESIAN_POINT('',(1.,-4.,14.5));
#9773=CARTESIAN_POINT('Origin',(0.,-4.,14.5));
#9774=CARTESIAN_POINT('',(1.,-4.,8.5));
#9775=CARTESIAN_POINT('Origin',(-1.,0.,14.5));
#9776=CARTESIAN_POINT('',(-1.,-6.,6.5));
#9777=CARTESIAN_POINT('',(-1.,0.,6.5));
#9778=CARTESIAN_POINT('',(-1.,-6.,14.5));
#9779=CARTESIAN_POINT('',(-1.,-6.,6.5));
#9780=CARTESIAN_POINT('',(-1.,0.,14.5));
#9781=CARTESIAN_POINT('Origin',(0.,0.,6.5));
#9782=CARTESIAN_POINT('',(1.,-6.,6.5));
#9783=CARTESIAN_POINT('',(1.,0.,6.5));
#9784=CARTESIAN_POINT('Origin',(0.,-6.,6.5));
#9785=CARTESIAN_POINT('Origin',(0.,0.,14.5));
#9786=CARTESIAN_POINT('',(1.,-6.,14.5));
#9787=CARTESIAN_POINT('Origin',(0.,-6.,14.5));
#9788=CARTESIAN_POINT('',(1.,0.,14.5));
#9789=CARTESIAN_POINT('Origin',(1.,0.,6.5));
#9790=CARTESIAN_POINT('',(1.,-6.,14.5));
#9791=CARTESIAN_POINT('Origin',(0.,-6.,10.5));
#9792=CARTESIAN_POINT('',(0.,0.,-2.5));
#9793=CARTESIAN_POINT('',(0.,0.,0.));
#9794=CARTESIAN_POINT('',(0.,0.,0.));
#9795=CARTESIAN_POINT('',(0.,0.,0.));
#9796=CARTESIAN_POINT('',(0.,0.,0.));
#9797=CARTESIAN_POINT('',(0.,0.,0.));
#9798=CARTESIAN_POINT('',(0.,0.,0.));
#9799=CARTESIAN_POINT('',(0.,0.,0.));
#9800=CARTESIAN_POINT('',(0.,0.,0.));
#9801=UNCERTAINTY_MEASURE_WITH_UNIT(LENGTH_MEASURE(0.01),#9823,
'DISTANCE_ACCURACY_VALUE',
'Maximum model space distance between geometric entities at asserted c
onnectivities');
#9802=UNCERTAINTY_MEASURE_WITH_UNIT(LENGTH_MEASURE(0.01),#9823,
'DISTANCE_ACCURACY_VALUE',
'Maximum model space distance between geometric entities at asserted c
onnectivities');
#9803=UNCERTAINTY_MEASURE_WITH_UNIT(LENGTH_MEASURE(0.01),#9823,
'DISTANCE_ACCURACY_VALUE',
'Maximum model space distance between geometric entities at asserted c
onnectivities');
#9804=UNCERTAINTY_MEASURE_WITH_UNIT(LENGTH_MEASURE(0.01),#9823,
'DISTANCE_ACCURACY_VALUE',
'Maximum model space distance between geometric entities at asserted c
onnectivities');
#9805=UNCERTAINTY_MEASURE_WITH_UNIT(LENGTH_MEASURE(0.01),#9823,
'DISTANCE_ACCURACY_VALUE',
'Maximum model space distance between geometric entities at asserted c
onnectivities');
#9806=UNCERTAINTY_MEASURE_WITH_UNIT(LENGTH_MEASURE(0.01),#9823,
'DISTANCE_ACCURACY_VALUE',
'Maximum model space distance between geometric entities at asserted c
onnectivities');
#9807=UNCERTAINTY_MEASURE_WITH_UNIT(LENGTH_MEASURE(0.01),#9823,
'DISTANCE_ACCURACY_VALUE',
'Maximum model space distance between geometric entities at asserted c
onnectivities');
#9808=UNCERTAINTY_MEASURE_WITH_UNIT(LENGTH_MEASURE(0.01),#9823,
'DISTANCE_ACCURACY_VALUE',
'Maximum model space distance between geometric entities at asserted c
onnectivities');
#9809=UNCERTAINTY_MEASURE_WITH_UNIT(LENGTH_MEASURE(0.01),#9823,
'DISTANCE_ACCURACY_VALUE',
'Maximum model space distance between geometric entities at asserted c
onnectivities');
#9810=UNCERTAINTY_MEASURE_WITH_UNIT(LENGTH_MEASURE(0.01),#9823,
'DISTANCE_ACCURACY_VALUE',
'Maximum model space distance between geometric entities at asserted c
onnectivities');
#9811=UNCERTAINTY_MEASURE_WITH_UNIT(LENGTH_MEASURE(0.01),#9823,
'DISTANCE_ACCURACY_VALUE',
'Maximum model space distance between geometric entities at asserted c
onnectivities');
#9812=(
GEOMETRIC_REPRESENTATION_CONTEXT(3)
GLOBAL_UNCERTAINTY_ASSIGNED_CONTEXT((#9801))
GLOBAL_UNIT_ASSIGNED_CONTEXT((#9823,#9825,#9826))
REPRESENTATION_CONTEXT('','3D')
);
#9813=(
GEOMETRIC_REPRESENTATION_CONTEXT(3)
GLOBAL_UNCERTAINTY_ASSIGNED_CONTEXT((#9802))
GLOBAL_UNIT_ASSIGNED_CONTEXT((#9823,#9825,#9826))
REPRESENTATION_CONTEXT('','3D')
);
#9814=(
GEOMETRIC_REPRESENTATION_CONTEXT(3)
GLOBAL_UNCERTAINTY_ASSIGNED_CONTEXT((#9803))
GLOBAL_UNIT_ASSIGNED_CONTEXT((#9823,#9825,#9826))
REPRESENTATION_CONTEXT('','3D')
);
#9815=(
GEOMETRIC_REPRESENTATION_CONTEXT(3)
GLOBAL_UNCERTAINTY_ASSIGNED_CONTEXT((#9804))
GLOBAL_UNIT_ASSIGNED_CONTEXT((#9823,#9825,#9826))
REPRESENTATION_CONTEXT('','3D')
);
#9816=(
GEOMETRIC_REPRESENTATION_CONTEXT(3)
GLOBAL_UNCERTAINTY_ASSIGNED_CONTEXT((#9805))
GLOBAL_UNIT_ASSIGNED_CONTEXT((#9823,#9825,#9826))
REPRESENTATION_CONTEXT('','3D')
);
#9817=(
GEOMETRIC_REPRESENTATION_CONTEXT(3)
GLOBAL_UNCERTAINTY_ASSIGNED_CONTEXT((#9806))
GLOBAL_UNIT_ASSIGNED_CONTEXT((#9823,#9825,#9826))
REPRESENTATION_CONTEXT('','3D')
);
#9818=(
GEOMETRIC_REPRESENTATION_CONTEXT(3)
GLOBAL_UNCERTAINTY_ASSIGNED_CONTEXT((#9807))
GLOBAL_UNIT_ASSIGNED_CONTEXT((#9823,#9825,#9826))
REPRESENTATION_CONTEXT('','3D')
);
#9819=(
GEOMETRIC_REPRESENTATION_CONTEXT(3)
GLOBAL_UNCERTAINTY_ASSIGNED_CONTEXT((#9808))
GLOBAL_UNIT_ASSIGNED_CONTEXT((#9823,#9825,#9826))
REPRESENTATION_CONTEXT('','3D')
);
#9820=(
GEOMETRIC_REPRESENTATION_CONTEXT(3)
GLOBAL_UNCERTAINTY_ASSIGNED_CONTEXT((#9809))
GLOBAL_UNIT_ASSIGNED_CONTEXT((#9823,#9825,#9826))
REPRESENTATION_CONTEXT('','3D')
);
#9821=(
GEOMETRIC_REPRESENTATION_CONTEXT(3)
GLOBAL_UNCERTAINTY_ASSIGNED_CONTEXT((#9810))
GLOBAL_UNIT_ASSIGNED_CONTEXT((#9823,#9825,#9826))
REPRESENTATION_CONTEXT('','3D')
);
#9822=(
GEOMETRIC_REPRESENTATION_CONTEXT(3)
GLOBAL_UNCERTAINTY_ASSIGNED_CONTEXT((#9811))
GLOBAL_UNIT_ASSIGNED_CONTEXT((#9823,#9825,#9826))
REPRESENTATION_CONTEXT('','3D')
);
#9823=(
LENGTH_UNIT()
NAMED_UNIT(*)
SI_UNIT(.MILLI.,.METRE.)
);
#9824=(
LENGTH_UNIT()
NAMED_UNIT(*)
SI_UNIT($,.METRE.)
);
#9825=(
NAMED_UNIT(*)
PLANE_ANGLE_UNIT()
SI_UNIT($,.RADIAN.)
);
#9826=(
NAMED_UNIT(*)
SI_UNIT($,.STERADIAN.)
SOLID_ANGLE_UNIT()
);
#9827=SHAPE_DEFINITION_REPRESENTATION(#9837,#9856);
#9828=SHAPE_DEFINITION_REPRESENTATION(#9838,#9857);
#9829=SHAPE_DEFINITION_REPRESENTATION(#9839,#9858);
#9830=SHAPE_DEFINITION_REPRESENTATION(#9840,#9859);
#9831=SHAPE_DEFINITION_REPRESENTATION(#9841,#9860);
#9832=SHAPE_DEFINITION_REPRESENTATION(#9842,#9861);
#9833=SHAPE_DEFINITION_REPRESENTATION(#9843,#9862);
#9834=SHAPE_DEFINITION_REPRESENTATION(#9844,#9863);
#9835=SHAPE_DEFINITION_REPRESENTATION(#9845,#9864);
#9836=SHAPE_DEFINITION_REPRESENTATION(#9846,#9865);
#9837=PRODUCT_DEFINITION_SHAPE('',$,#9867);
#9838=PRODUCT_DEFINITION_SHAPE('',$,#9868);
#9839=PRODUCT_DEFINITION_SHAPE('',$,#9869);
#9840=PRODUCT_DEFINITION_SHAPE('',$,#9870);
#9841=PRODUCT_DEFINITION_SHAPE('',$,#9871);
#9842=PRODUCT_DEFINITION_SHAPE('',$,#9872);
#9843=PRODUCT_DEFINITION_SHAPE('',$,#9873);
#9844=PRODUCT_DEFINITION_SHAPE('',$,#9874);
#9845=PRODUCT_DEFINITION_SHAPE('',$,#9875);
#9846=PRODUCT_DEFINITION_SHAPE('',$,#9876);
#9847=PRODUCT_DEFINITION_SHAPE($,$,#38);
#9848=PRODUCT_DEFINITION_SHAPE($,$,#39);
#9849=PRODUCT_DEFINITION_SHAPE($,$,#40);
#9850=PRODUCT_DEFINITION_SHAPE($,$,#41);
#9851=PRODUCT_DEFINITION_SHAPE($,$,#42);
#9852=PRODUCT_DEFINITION_SHAPE($,$,#43);
#9853=PRODUCT_DEFINITION_SHAPE($,$,#44);
#9854=PRODUCT_DEFINITION_SHAPE($,$,#45);
#9855=PRODUCT_DEFINITION_SHAPE($,$,#46);
#9856=SHAPE_REPRESENTATION('',(#3397,#3718,#3719,#3720,#3721,#3722,#3723,
#3724,#3725,#3726),#9812);
#9857=SHAPE_REPRESENTATION('',(#3398),#9813);
#9858=SHAPE_REPRESENTATION('',(#3488),#9814);
#9859=SHAPE_REPRESENTATION('',(#3566),#9815);
#9860=SHAPE_REPRESENTATION('',(#3644),#9816);
#9861=SHAPE_REPRESENTATION('',(#3657),#9817);
#9862=SHAPE_REPRESENTATION('',(#3670),#9818);
#9863=SHAPE_REPRESENTATION('',(#3683),#9819);
#9864=SHAPE_REPRESENTATION('',(#3696),#9820);
#9865=SHAPE_REPRESENTATION('',(#3707),#9821);
#9866=PRODUCT_DEFINITION_CONTEXT('part definition',#9898,'design');
#9867=PRODUCT_DEFINITION('BR-255','BR-255',#9877,#9866);
#9868=PRODUCT_DEFINITION('Spider','Spider',#9878,#9866);
#9869=PRODUCT_DEFINITION('Hub_01','Hub_01',#9879,#9866);
#9870=PRODUCT_DEFINITION('Hub_02','Hub_02',#9880,#9866);
#9871=PRODUCT_DEFINITION('Screw_01','Screw_01',#9881,#9866);
#9872=PRODUCT_DEFINITION('Screw_02','Screw_02',#9882,#9866);
#9873=PRODUCT_DEFINITION('Rod','Rod',#9883,#9866);
#9874=PRODUCT_DEFINITION('Rod_02','Rod_02',#9884,#9866);
#9875=PRODUCT_DEFINITION('Pin_02','Pin_02',#9885,#9866);
#9876=PRODUCT_DEFINITION('Pin_01','Pin_01',#9886,#9866);
#9877=PRODUCT_DEFINITION_FORMATION('',$,#9900);
#9878=PRODUCT_DEFINITION_FORMATION('',$,#9901);
#9879=PRODUCT_DEFINITION_FORMATION('',$,#9902);
#9880=PRODUCT_DEFINITION_FORMATION('',$,#9903);
#9881=PRODUCT_DEFINITION_FORMATION('',$,#9904);
#9882=PRODUCT_DEFINITION_FORMATION('',$,#9905);
#9883=PRODUCT_DEFINITION_FORMATION('',$,#9906);
#9884=PRODUCT_DEFINITION_FORMATION('',$,#9907);
#9885=PRODUCT_DEFINITION_FORMATION('',$,#9908);
#9886=PRODUCT_DEFINITION_FORMATION('',$,#9909);
#9887=PRODUCT_RELATED_PRODUCT_CATEGORY('BR-255','BR-255',(#9900));
#9888=PRODUCT_RELATED_PRODUCT_CATEGORY('Spider','Spider',(#9901));
#9889=PRODUCT_RELATED_PRODUCT_CATEGORY('Hub_01','Hub_01',(#9902));
#9890=PRODUCT_RELATED_PRODUCT_CATEGORY('Hub_02','Hub_02',(#9903));
#9891=PRODUCT_RELATED_PRODUCT_CATEGORY('Screw_01','Screw_01',(#9904));
#9892=PRODUCT_RELATED_PRODUCT_CATEGORY('Screw_02','Screw_02',(#9905));
#9893=PRODUCT_RELATED_PRODUCT_CATEGORY('Rod','Rod',(#9906));
#9894=PRODUCT_RELATED_PRODUCT_CATEGORY('Rod_02','Rod_02',(#9907));
#9895=PRODUCT_RELATED_PRODUCT_CATEGORY('Pin_02','Pin_02',(#9908));
#9896=PRODUCT_RELATED_PRODUCT_CATEGORY('Pin_01','Pin_01',(#9909));
#9897=APPLICATION_PROTOCOL_DEFINITION('international standard',
'automotive_design',2009,#9898);
#9898=APPLICATION_CONTEXT(
'Core Data for Automotive Mechanical Design Process');
#9899=PRODUCT_CONTEXT('part definition',#9898,'mechanical');
#9900=PRODUCT('BR-255','BR-255',$,(#9899));
#9901=PRODUCT('Spider','Spider',
'Spur Gear; Module: 3.0; Num Teeth: 6; Pressure Angle: 20.0; Backlash:
 0.00 mm',(#9899));
#9902=PRODUCT('Hub_01','Hub_01',$,(#9899));
#9903=PRODUCT('Hub_02','Hub_02',$,(#9899));
#9904=PRODUCT('Screw_01','Screw_01',$,(#9899));
#9905=PRODUCT('Screw_02','Screw_02',$,(#9899));
#9906=PRODUCT('Rod','Rod',$,(#9899));
#9907=PRODUCT('Rod_02','Rod_02',$,(#9899));
#9908=PRODUCT('Pin_02','Pin_02',$,(#9899));
#9909=PRODUCT('Pin_01','Pin_01',$,(#9899));
#9910=PRESENTATION_STYLE_ASSIGNMENT((#9913));
#9911=PRESENTATION_STYLE_ASSIGNMENT((#9914));
#9912=PRESENTATION_STYLE_ASSIGNMENT((#9915));
#9913=SURFACE_STYLE_USAGE(.BOTH.,#9916);
#9914=SURFACE_STYLE_USAGE(.BOTH.,#9917);
#9915=SURFACE_STYLE_USAGE(.BOTH.,#9918);
#9916=SURFACE_SIDE_STYLE('',(#9919));
#9917=SURFACE_SIDE_STYLE('',(#9920));
#9918=SURFACE_SIDE_STYLE('',(#9921));
#9919=SURFACE_STYLE_FILL_AREA(#9922);
#9920=SURFACE_STYLE_FILL_AREA(#9923);
#9921=SURFACE_STYLE_FILL_AREA(#9924);
#9922=FILL_AREA_STYLE('Steel - Satin',(#9925));
#9923=FILL_AREA_STYLE('Opaque(78,78,78)',(#9926));
#9924=FILL_AREA_STYLE('Opaque(233,233,233)',(#9927));
#9925=FILL_AREA_STYLE_COLOUR('Steel - Satin',#9928);
#9926=FILL_AREA_STYLE_COLOUR('Opaque(78,78,78)',#9929);
#9927=FILL_AREA_STYLE_COLOUR('Opaque(233,233,233)',#9930);
#9928=COLOUR_RGB('Steel - Satin', 0.09019608, 0.27058824, 0.51372549);
#9929=COLOUR_RGB('Opaque(78,78,78)', 0.09019608, 0.27058824, 0.51372549);
#9930=COLOUR_RGB('Opaque(233,233,233)', 0.40784314, 0.44705882, 0.49803922);
ENDSEC;
END-ISO-10303-21;
